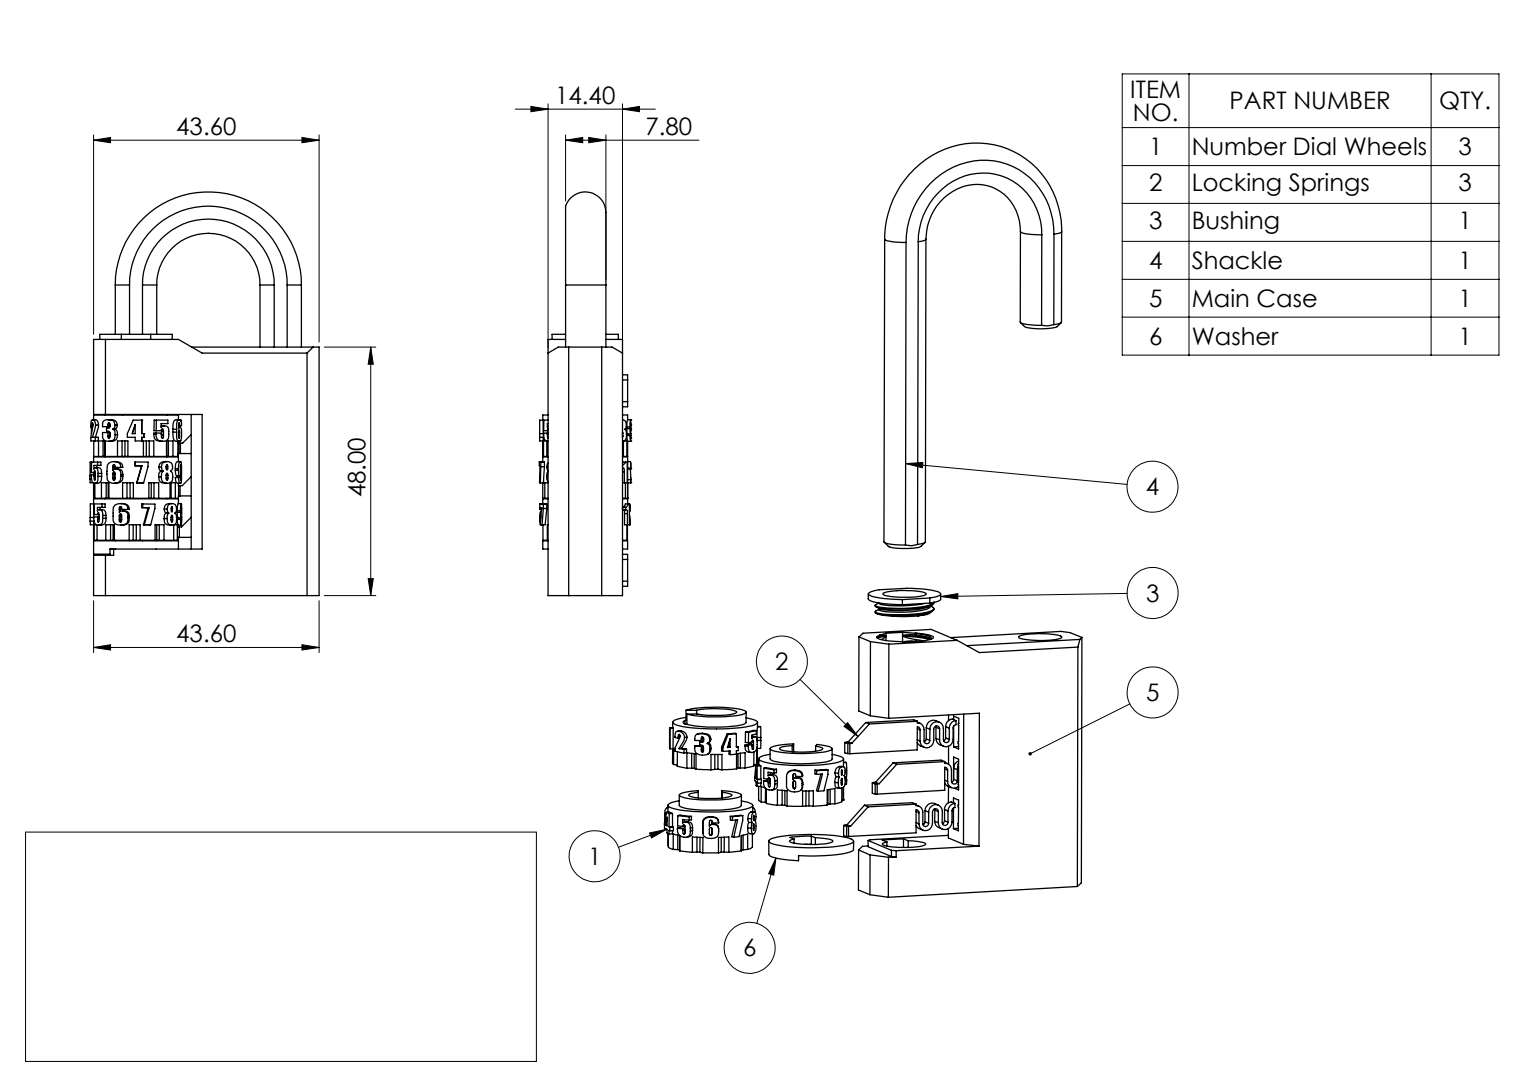
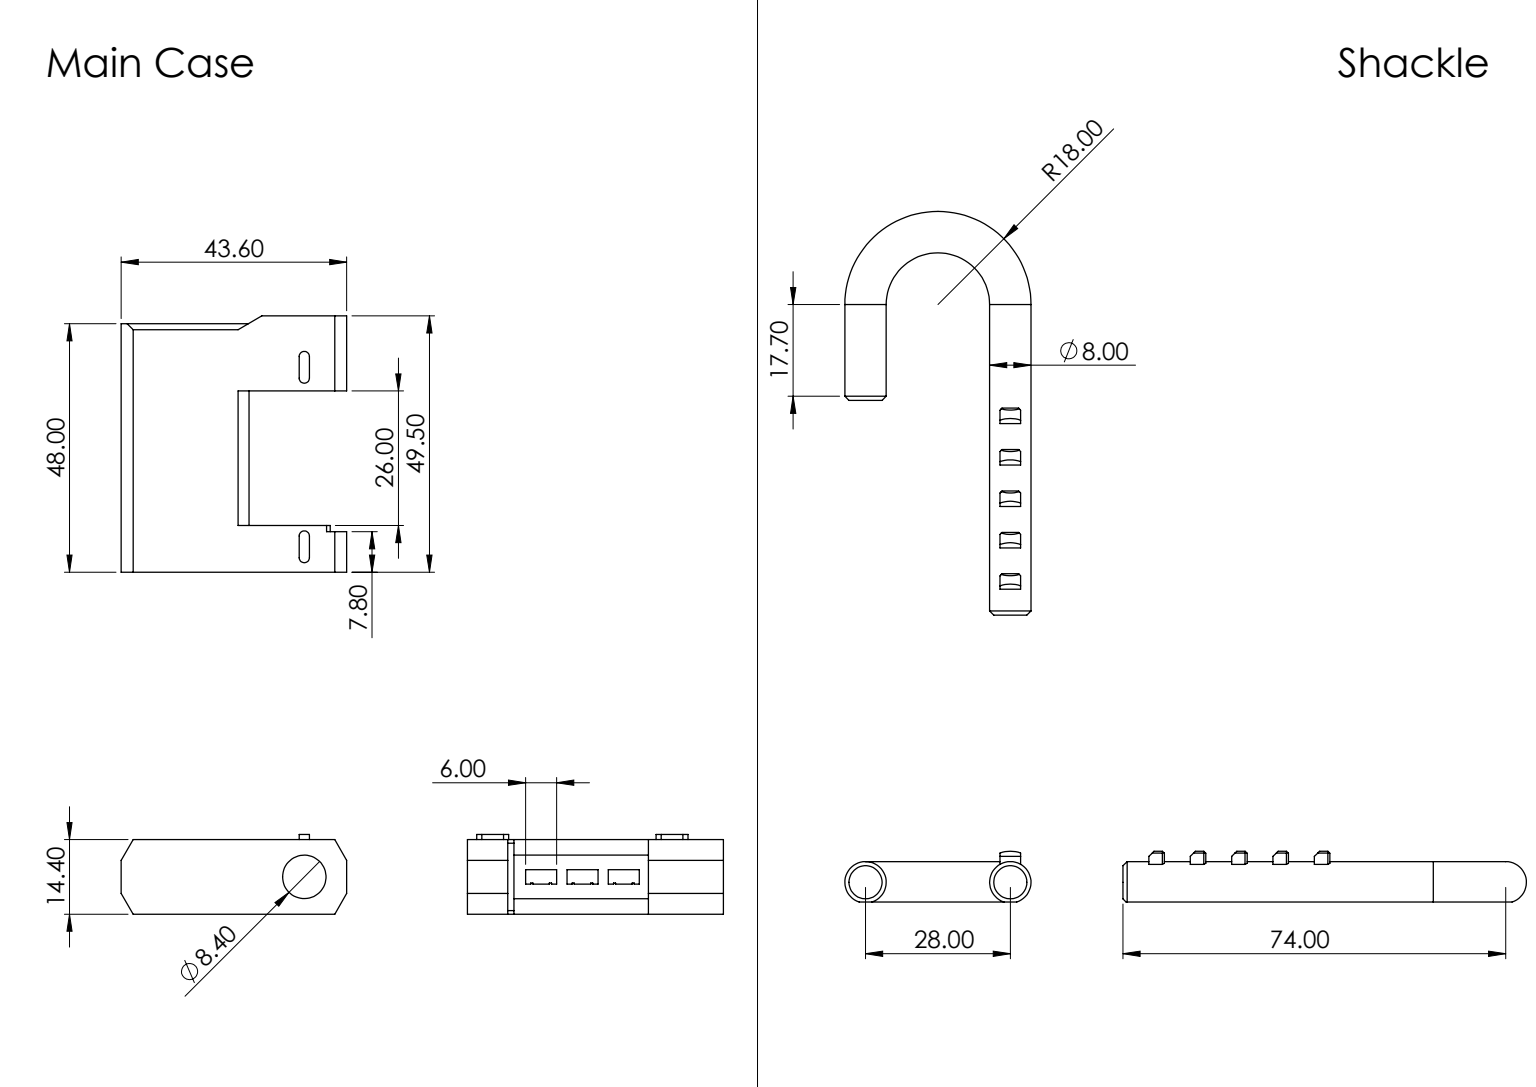
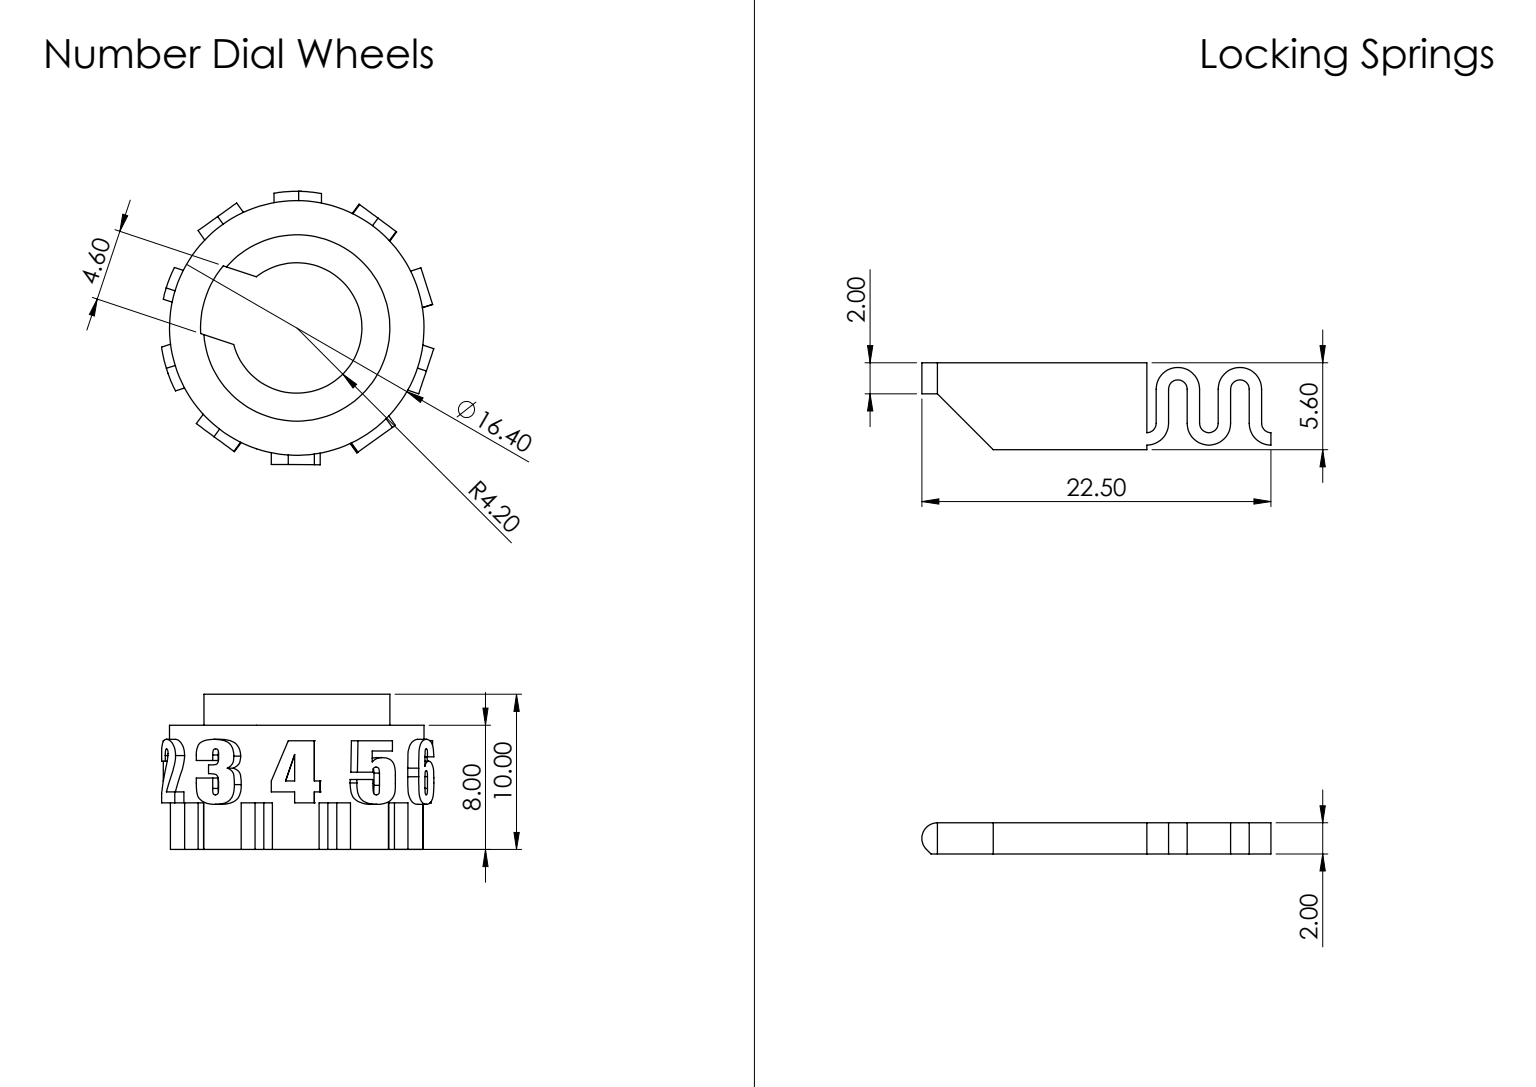
ISO-10303-21;
HEADER;
FILE_DESCRIPTION (('STEP AP214'),
    '1' );
FILE_NAME ('MAS-160',
    '2026-10-06T10:59:17',
    ( '' ),
    ( '' ),
    'SwSTEP 2.0',
    'SolidWorks 2026',
    '' );
FILE_SCHEMA (( 'AUTOMOTIVE_DESIGN' ));
ENDSEC;

DATA;
#1 = CARTESIAN_POINT ( 'NONE',  ( -5.668520211720758262, 50.55432463793220421, 79.06611278947218580 ) ) ;
#2 = EDGE_CURVE ( 'NONE', #13018, #165, #5489, .T. ) ;
#3 = DIRECTION ( 'NONE',  ( -0.007885122365275663500, -0.9999689119394085113, -1.805443505845543142E-16 ) ) ;
#4 = VECTOR ( 'NONE', #1471, 1000.000000000000000 ) ;
#5 = CIRCLE ( 'NONE', #15294, 8.199999999999995737 ) ;
#6 = CARTESIAN_POINT ( 'NONE',  ( -5.044287576081563529, 45.27497882680665242, 92.45433879953097289 ) ) ;
#7 = EDGE_CURVE ( 'NONE', #18543, #18148, #5615, .T. ) ;
#8 = EDGE_CURVE ( 'NONE', #10795, #13483, #5393, .T. ) ;
#9 = CARTESIAN_POINT ( 'NONE',  ( 9.261243355884198891, 42.55025836209524215, 77.91040118276930571 ) ) ;
#10 = ORIENTED_EDGE ( 'NONE', *, *, #4967, .T. ) ;
#11 = CARTESIAN_POINT ( 'NONE',  ( 0.5922110576113025493, 52.20739479508054615, 75.36022115247205022 ) ) ;
#12 = CARTESIAN_POINT ( 'NONE',  ( 4.579592178280777581, 52.10552964593085790, 78.58658920843723195 ) ) ;
#13 = CARTESIAN_POINT ( 'NONE',  ( -4.517072128342570991, 36.94403992325788977, 76.53375056423675460 ) ) ;
#14 = DIRECTION ( 'NONE',  ( -5.084437235940625660E-16, 1.000000000000000000, 0.000000000000000000 ) ) ;
#15 = CARTESIAN_POINT ( 'NONE',  ( 13.32277635493562684, 36.96218137147968008, 93.55433879953098142 ) ) ;
#16 = ORIENTED_EDGE ( 'NONE', *, *, #17837, .F. ) ;
#17 = CARTESIAN_POINT ( 'NONE',  ( -4.383821200644077543, 51.47232351541473605, 78.52322435057745054 ) ) ;
#18 = ORIENTED_EDGE ( 'NONE', *, *, #1917, .T. ) ;
#19 = CARTESIAN_POINT ( 'NONE',  ( 6.198496396448986090, 45.68315280215533392, 92.83621380123798872 ) ) ;
#20 = VECTOR ( 'NONE', #2644, 1000.000000000000000 ) ;
#21 = DIRECTION ( 'NONE',  ( -0.9534635866061492715, -0.3015081906286096181, -2.009271279954799034E-16 ) ) ;
#22 = DIRECTION ( 'NONE',  ( 1.000000000000000000, 1.402518428993831676E-16, 0.000000000000000000 ) ) ;
#23 = FACE_OUTER_BOUND ( 'NONE', #2715, .T. ) ;
#24 = PRODUCT_DEFINITION_SHAPE ( 'NONE', 'NONE',  #21038 ) ;
#25 = CARTESIAN_POINT ( 'NONE',  ( 11.22215374030650281, 42.76218137147968434, 61.80715055817104542 ) ) ;
#26 = VERTEX_POINT ( 'NONE', #13599 ) ;
#27 = CARTESIAN_POINT ( 'NONE',  ( 4.987972048783305468, 51.80387588613526617, 77.70137231118654597 ) ) ;
#28 = ORIENTED_EDGE ( 'NONE', *, *, #6498, .T. ) ;
#29 = DIRECTION ( 'NONE',  ( -1.402518428993831183E-16, 1.000000000000000000, -3.469446951953617640E-16 ) ) ;
#30 = EDGE_CURVE ( 'NONE', #19399, #15803, #16589, .T. ) ;
#31 = CARTESIAN_POINT ( 'NONE',  ( -4.567115856812060670, 47.10047254335474065, 90.96121380123797451 ) ) ;
#32 = PRODUCT_DEFINITION_FORMATION_WITH_SPECIFIED_SOURCE ( 'ANY', '', #540, .NOT_KNOWN. ) ;
#33 = DIRECTION ( 'NONE',  ( -1.000000000000000000, 0.000000000000000000, 0.000000000000000000 ) ) ;
#34 =( BOUNDED_CURVE ( )  B_SPLINE_CURVE ( 2, ( #7482, #18864, #675, #2170, #8669, #8881, #884, #11966, #2587, #10382, #10705 ),
 .UNSPECIFIED., .F., .F. ) 
 B_SPLINE_CURVE_WITH_KNOTS ( ( 3, 2, 2, 2, 2, 3 ),
 ( 0.5133705948588321855, 0.5208165094390924121, 0.5468573349110280590, 0.5728981603829637059, 0.5989389858548992418, 0.6196804601785050881 ),
 .UNSPECIFIED. ) 
 CURVE ( )  GEOMETRIC_REPRESENTATION_ITEM ( )  RATIONAL_B_SPLINE_CURVE ( ( 0.9689162004317901644, 0.9782346953885442398, 1.000000000000000000, 0.9238795325112867385, 1.000000000000000000, 0.9238795325112867385, 1.000000000000000000, 0.9238795325112867385, 1.000000000000000000, 0.9393701738211195362, 0.9753234597474376155 ) ) 
 REPRESENTATION_ITEM ( '' )  );
#35 = ORIENTED_EDGE ( 'NONE', *, *, #1554, .F. ) ;
#36 = DIRECTION ( 'NONE',  ( -0.5941461771851783702, -0.8043570849667693867, -2.357623395011398763E-16 ) ) ;
#37 = DIRECTION ( 'NONE',  ( 1.000000000000000000, 0.000000000000000000, 0.000000000000000000 ) ) ;
#38 = CARTESIAN_POINT ( 'NONE',  ( 5.756838674491786101, 51.23594508156129734, 75.97260389846793771 ) ) ;
#39 = CARTESIAN_POINT ( 'NONE',  ( -1.214884381343047881, 47.76843358786783966, 61.41730067788144964 ) ) ;
#40 = PLANE ( 'NONE',  #3794 ) ;
#41 = ORIENTED_EDGE ( 'NONE', *, *, #20258, .F. ) ;
#42 = CARTESIAN_POINT ( 'NONE',  ( -4.383767596367525776, 51.47236181906818331, 76.38961819735682468 ) ) ;
#43 = DIRECTION ( 'NONE',  ( -1.402518428993830937E-16, 1.000000000000000000, -3.469446951953617147E-16 ) ) ;
#44 = ORIENTED_EDGE ( 'NONE', *, *, #9004, .T. ) ;
#45 = CARTESIAN_POINT ( 'NONE',  ( 4.947340820402381212, 51.83388853781453776, 77.72408214165703555 ) ) ;
#46 = CARTESIAN_POINT ( 'NONE',  ( -7.770838052284047670, 41.18381739692070198, 76.59276269229415846 ) ) ;
#47 = FACE_OUTER_BOUND ( 'NONE', #1899, .T. ) ;
#48 = CARTESIAN_POINT ( 'NONE',  ( -3.467962453771610498, 40.50591351489412517, 91.93871379611699979 ) ) ;
#49 = VECTOR ( 'NONE', #11838, 1000.000000000000000 ) ;
#50 = CARTESIAN_POINT ( 'NONE',  ( -4.705149740856862550, 37.08296527939383935, 78.93669174070734584 ) ) ;
#51 = AXIS2_PLACEMENT_3D ( 'NONE', #3757, #13451, #252 ) ;
#52 = CARTESIAN_POINT ( 'NONE',  ( 11.22215374030650281, 45.56218137147968861, 78.80433879953099563 ) ) ;
#53 = CARTESIAN_POINT ( 'NONE',  ( -3.095340769291234473, 36.81869718614577636, 77.24173421363296654 ) ) ;
#54 = VERTEX_POINT ( 'NONE', #8619 ) ;
#55 = CARTESIAN_POINT ( 'NONE',  ( 27.03948732994508219, 45.16218137147969003, 73.00433879953099847 ) ) ;
#56 = CARTESIAN_POINT ( 'NONE',  ( -3.319090015466918064, 36.97315379936787849, 77.82155188814751057 ) ) ;
#57 = VERTEX_POINT ( 'NONE', #8931 ) ;
#58 = CARTESIAN_POINT ( 'NONE',  ( -8.080917653967048864, 42.28401339625642663, 76.87634113524943302 ) ) ;
#59 = DIRECTION ( 'NONE',  ( -0.5813877811927011807, 0.8136266022444372803, 5.636455622144619183E-17 ) ) ;
#60 = CARTESIAN_POINT ( 'NONE',  ( 9.342575031381675998, 42.79401455314646086, 78.75800315165874110 ) ) ;
#61 = ORIENTED_EDGE ( 'NONE', *, *, #4152, .T. ) ;
#62 = CARTESIAN_POINT ( 'NONE',  ( -1.876873622437039701, 39.01745058958429269, 93.96996379782397923 ) ) ;
#63 = CARTESIAN_POINT ( 'NONE',  ( -5.888951387225215939, 37.95739186912707197, 75.98496980016291502 ) ) ;
#64 = EDGE_LOOP ( 'NONE', ( #4003, #6865, #2890, #187 ) ) ;
#65 = CIRCLE ( 'NONE', #13313, 4.200000000000000178 ) ;
#66 = CARTESIAN_POINT ( 'NONE',  ( 11.22215374030649926, 45.56218137147968861, 78.80433879953099563 ) ) ;
#67 = CARTESIAN_POINT ( 'NONE',  ( 2.522153740306511072, 49.16218137147969003, 50.55433879953100273 ) ) ;
#68 = CARTESIAN_POINT ( 'NONE',  ( -0.8237052942265477018, 49.18499566818285018, 93.69558879953099506 ) ) ;
#69 = CIRCLE ( 'NONE', #12653, 8.199999999999999289 ) ;
#70 = ORIENTED_EDGE ( 'NONE', *, *, #17800, .F. ) ;
#71 = CARTESIAN_POINT ( 'NONE',  ( 4.142779209164833887, 51.51417078508897163, 78.58658920843723195 ) ) ;
#72 = CARTESIAN_POINT ( 'NONE',  ( -4.555118767358855791, 36.97214344288707366, 78.05402056118774112 ) ) ;
#73 = ORIENTED_EDGE ( 'NONE', *, *, #14534, .T. ) ;
#74 = CARTESIAN_POINT ( 'NONE',  ( -7.805021908755670701, 41.31633897062200589, 78.88165831555673435 ) ) ;
#75 = DIRECTION ( 'NONE',  ( 1.334402673828313339E-16, 1.871524341742854397E-32, -1.000000000000000000 ) ) ;
#76 = ADVANCED_FACE ( 'NONE', ( #16800 ), #11914, .T. ) ;
#77 = CARTESIAN_POINT ( 'NONE',  ( 2.122153740306496505, 47.82824192744437397, 69.55433879953100984 ) ) ;
#78 = AXIS2_PLACEMENT_3D ( 'NONE', #12417, #15502, #20488 ) ;
#79 = CARTESIAN_POINT ( 'NONE',  ( 0.3449000470298889676, 52.34510639596846460, 77.07502437766733294 ) ) ;
#80 = CARTESIAN_POINT ( 'NONE',  ( 0.5221537403065104055, 40.36218137147969998, 46.15433879953098284 ) ) ;
#81 = VECTOR ( 'NONE', #12886, 999.9999999999998863 ) ;
#82 = ORIENTED_EDGE ( 'NONE', *, *, #15786, .F. ) ;
#83 = CARTESIAN_POINT ( 'NONE',  ( -5.510184220575293779, 38.60782276366593635, 76.52855510524061344 ) ) ;
#84 = CARTESIAN_POINT ( 'NONE',  ( 9.340212240349364592, 42.78693311852996572, 76.09591779779900378 ) ) ;
#85 = CARTESIAN_POINT ( 'NONE',  ( 8.299662904660788598, 41.56403757284476796, 75.97198585835440099 ) ) ;
#86 = CARTESIAN_POINT ( 'NONE',  ( 1.695410614910025870, 52.88397731476800345, 79.31282343688214098 ) ) ;
#87 = ORIENTED_EDGE ( 'NONE', *, *, #18743, .F. ) ;
#88 = CARTESIAN_POINT ( 'NONE',  ( 5.873814141894775354, 51.14954001584995069, 78.86250487280319987 ) ) ;
#89 = ORIENTED_EDGE ( 'NONE', *, *, #15661, .F. ) ;
#90 = AXIS2_PLACEMENT_3D ( 'NONE', #13292, #19764, #11704 ) ;
#91 = VECTOR ( 'NONE', #3485, 1000.000000000000114 ) ;
#92 = CARTESIAN_POINT ( 'NONE',  ( 0.5221537403065010796, 44.16218137147969003, 54.55433879953099563 ) ) ;
#93 =( LENGTH_UNIT ( ) NAMED_UNIT ( * ) SI_UNIT ( .MILLI., .METRE. ) );
#94 = CARTESIAN_POINT ( 'NONE',  ( 5.077155773762835445, 37.34368029226138219, 77.47144026546204998 ) ) ;
#95 = ADVANCED_FACE ( 'NONE', ( #11803 ), #8817, .F. ) ;
#96 = LINE ( 'NONE', #16272, #3476 ) ;
#97 = CARTESIAN_POINT ( 'NONE',  ( 5.856396280011940014, 46.10368687828906076, 93.18871379782397923 ) ) ;
#98 = CARTESIAN_POINT ( 'NONE',  ( 32.52215374030649286, 44.16218137147969003, 105.5543387995310098 ) ) ;
#99 = CARTESIAN_POINT ( 'NONE',  ( 6.470280134917119064, 49.78412166693355800, 77.24227907682649175 ) ) ;
#100 = CARTESIAN_POINT ( 'NONE',  ( 4.485821066275814673, 51.34094918448491995, 77.76180969966527812 ) ) ;
#101 = CARTESIAN_POINT ( 'NONE',  ( 5.384092268968043271, 50.76532863195453160, 75.97198585835440099 ) ) ;
#102 = CARTESIAN_POINT ( 'NONE',  ( -3.350035803220276609, 49.20851703305431357, 90.72683880123797451 ) ) ;
#103 = ORIENTED_EDGE ( 'NONE', *, *, #5988, .T. ) ;
#104 = CARTESIAN_POINT ( 'NONE',  ( -5.234090592717892676, 38.40967907571953077, 79.34222993022952153 ) ) ;
#105 = AXIS2_PLACEMENT_3D ( 'NONE', #8174, #11698, #19756 ) ;
#106 = EDGE_CURVE ( 'NONE', #5849, #17982, #8716, .T. ) ;
#107 = CARTESIAN_POINT ( 'NONE',  ( 8.951227662965957066, 41.62112166339042574, 78.59502675972919405 ) ) ;
#108 = CARTESIAN_POINT ( 'NONE',  ( -4.895593109503404428, 37.22363812428621088, 78.53742703482498655 ) ) ;
#109 = CARTESIAN_POINT ( 'NONE',  ( -1.477846259693489150, 50.16218137147969713, 53.15433879953100416 ) ) ;
#110 = CARTESIAN_POINT ( 'NONE',  ( 8.529329397667178014, 40.35666579756309602, 75.60774188071792423 ) ) ;
#111 = EDGE_LOOP ( 'NONE', ( #358, #7162, #18029, #16335 ) ) ;
#112 = CARTESIAN_POINT ( 'NONE',  ( 0.5218139128070994337, 52.20794990243870615, 75.36134551364482093 ) ) ;
#113 = CARTESIAN_POINT ( 'NONE',  ( 4.611645699796032893, 52.08185300078213942, 78.81874598975664981 ) ) ;
#114 = CARTESIAN_POINT ( 'NONE',  ( 7.692705115657170190, 40.18434116893706687, 78.65627992829327297 ) ) ;
#115 = DIRECTION ( 'NONE',  ( -1.000000000000000000, 0.000000000000000000, 0.000000000000000000 ) ) ;
#116 = CARTESIAN_POINT ( 'NONE',  ( -2.244031111076484120, 49.10779090901081645, 92.45433879953095868 ) ) ;
#117 = ORIENTED_EDGE ( 'NONE', *, *, #13949, .F. ) ;
#118 = ADVANCED_FACE ( 'NONE', ( #19767 ), #15314, .F. ) ;
#119 = CARTESIAN_POINT ( 'NONE',  ( -4.541431855014749885, 51.35970071229581180, 78.93463757479271692 ) ) ;
#120 = EDGE_CURVE ( 'NONE', #5204, #4614, #20185, .T. ) ;
#121 = VECTOR ( 'NONE', #9015, 1000.000000000000000 ) ;
#122 = VERTEX_POINT ( 'NONE', #18600 ) ;
#123 = CARTESIAN_POINT ( 'NONE',  ( -3.981178359372548492, 46.76218137147973408, 95.41433880294498238 ) ) ;
#124 = CARTESIAN_POINT ( 'NONE',  ( 4.359773538758245692, 47.36728266200564263, 95.05433879953096721 ) ) ;
#125 = CARTESIAN_POINT ( 'NONE',  ( -7.372207198384979066, 41.95818682111052311, 78.62287654527649750 ) ) ;
#126 = EDGE_CURVE ( 'NONE', #1287, #15187, #18942, .T. ) ;
#127 = CARTESIAN_POINT ( 'NONE',  ( 8.647256388514012571, 43.05630782556218605, 78.60052408832618198 ) ) ;
#128 = ORIENTED_EDGE ( 'NONE', *, *, #19583, .F. ) ;
#129 = VERTEX_POINT ( 'NONE', #13492 ) ;
#130 = AXIS2_PLACEMENT_3D ( 'NONE', #14597, #8214, #5004 ) ;
#131 = CARTESIAN_POINT ( 'NONE',  ( -1.477846259693492481, 49.81903562097207327, 69.15433879953098995 ) ) ;
#132 = CARTESIAN_POINT ( 'NONE',  ( -5.154188915835984375, 42.64120994080404614, 91.11746380123797451 ) ) ;
#133 = CARTESIAN_POINT ( 'NONE',  ( -3.350035803220276609, 49.20851703305431357, 94.47683880123798872 ) ) ;
#134 = ORIENTED_EDGE ( 'NONE', *, *, #20923, .T. ) ;
#135 = DIRECTION ( 'NONE',  ( 1.000000000000000000, 0.000000000000000000, 0.000000000000000000 ) ) ;
#136 = CARTESIAN_POINT ( 'NONE',  ( -5.850799091716242017, 37.92921030530281001, 79.12851299606570876 ) ) ;
#137 = CARTESIAN_POINT ( 'NONE',  ( 4.483628625085211539, 47.60909685017714565, 92.55433879953102405 ) ) ;
#138 = LINE ( 'NONE', #1946, #11877 ) ;
#139 = DIRECTION ( 'NONE',  ( 5.626130192357176673E-16, 1.831515347669941892E-30, -1.000000000000000000 ) ) ;
#140 = VERTEX_POINT ( 'NONE', #614 ) ;
#141 = CARTESIAN_POINT ( 'NONE',  ( -4.572866156349838285, 51.33723891144499163, 75.97260225988416948 ) ) ;
#142 = CARTESIAN_POINT ( 'NONE',  ( 1.514255888186003984, 52.36218137147968577, 83.03825919817350609 ) ) ;
#143 = ORIENTED_EDGE ( 'NONE', *, *, #10138, .T. ) ;
#144 = CARTESIAN_POINT ( 'NONE',  ( 4.577379499810326990, 52.10716406238486087, 78.43496551412393103 ) ) ;
#145 = ADVANCED_FACE ( 'NONE', ( #13399 ), #7094, .T. ) ;
#146 = CARTESIAN_POINT ( 'NONE',  ( -7.419359026272076996, 40.07233033562560109, 78.47931198110067896 ) ) ;
#147 = CARTESIAN_POINT ( 'NONE',  ( -5.170918566808907713, 50.90989255502720567, 75.43678921887351407 ) ) ;
#148 = CARTESIAN_POINT ( 'NONE',  ( -3.134114116279072437, 48.15229756555780227, 92.87621379611699979 ) ) ;
#149 = CARTESIAN_POINT ( 'NONE',  ( -5.616286711741430793, 44.43019146960381960, 93.73558879782397923 ) ) ;
#150 = LINE ( 'NONE', #6632, #10274 ) ;
#151 = ADVANCED_FACE ( 'NONE', ( #2321 ), #726, .T. ) ;
#152 = CARTESIAN_POINT ( 'NONE',  ( 3.722852957781953798, 40.32059543431686421, 95.05433879953096721 ) ) ;
#153 = ADVANCED_FACE ( 'NONE', ( #834 ), #13296, .T. ) ;
#154 = CARTESIAN_POINT ( 'NONE',  ( -3.501255140781828423, 36.19369683415101946, 76.91456057462045237 ) ) ;
#155 = ORIENTED_EDGE ( 'NONE', *, *, #1332, .F. ) ;
#156 = CARTESIAN_POINT ( 'NONE',  ( 0.6393167648259392433, 52.21315491623544602, 79.54845644658969661 ) ) ;
#157 = LINE ( 'NONE', #5245, #2424 ) ;
#158 = VERTEX_POINT ( 'NONE', #10219 ) ;
#159 = DIRECTION ( 'NONE',  ( 0.9485903129789495791, -0.3165065846431930341, 8.934458285744763183E-17 ) ) ;
#160 = DIRECTION ( 'NONE',  ( 1.193617070626243484E-16, 1.000000000000000000, 0.000000000000000000 ) ) ;
#161 = DIRECTION ( 'NONE',  ( -1.779391786395883536E-16, -5.922860397471806844E-17, 1.000000000000000000 ) ) ;
#162 = ORIENTED_EDGE ( 'NONE', *, *, #19825, .F. ) ;
#163 = PLANE ( 'NONE',  #17008 ) ;
#164 = CARTESIAN_POINT ( 'NONE',  ( -5.460139946343538497, 38.57665262741940637, 76.06004113464240390 ) ) ;
#165 = VERTEX_POINT ( 'NONE', #16122 ) ;
#166 = DIRECTION ( 'NONE',  ( 1.000000000000000000, 0.000000000000000000, 0.000000000000000000 ) ) ;
#167 = CARTESIAN_POINT ( 'NONE',  ( 0.7308905865242323330, 52.95996087887004933, 76.81167861208460579 ) ) ;
#168 = PLANE ( 'NONE',  #8612 ) ;
#169 = EDGE_LOOP ( 'NONE', ( #1521, #15928, #6222, #1148 ) ) ;
#170 = DIRECTION ( 'NONE',  ( -4.731737692062685363E-17, 0.7071067811865536790, 0.7071067811865414665 ) ) ;
#171 = CARTESIAN_POINT ( 'NONE',  ( -4.853788242550869825, 37.19275855307108003, 77.90854597583356167 ) ) ;
#172 = ORIENTED_EDGE ( 'NONE', *, *, #6800, .T. ) ;
#173 = DIRECTION ( 'NONE',  ( 1.540237394707284220E-16, 1.793354297423764243E-16, -1.000000000000000000 ) ) ;
#174 = CARTESIAN_POINT ( 'NONE',  ( 5.506586839745581941, 50.67343267475700941, 78.88820493356335817 ) ) ;
#175 = CARTESIAN_POINT ( 'NONE',  ( 1.314047178454490705, 52.92828027204963348, 75.43137060453751985 ) ) ;
#176 = CARTESIAN_POINT ( 'NONE',  ( 2.043125170982144745, 38.48583871533720213, 95.02371380123798872 ) ) ;
#177 = CARTESIAN_POINT ( 'NONE',  ( -43.61452724460164632, 45.75098584416670633, -16.20000000000000284 ) ) ;
#178 = EDGE_CURVE ( 'NONE', #3564, #14970, #12223, .T. ) ;
#179 = CARTESIAN_POINT ( 'NONE',  ( -4.518988042728760313, 37.69480848959909025, 76.08971211654539957 ) ) ;
#180 = CARTESIAN_POINT ( 'NONE',  ( 0.8326822781444389587, 52.96411479610753759, 76.79008513575435302 ) ) ;
#181 = CARTESIAN_POINT ( 'NONE',  ( 4.121594020068452657, 36.83821297622463220, 75.83703142516586126 ) ) ;
#182 = ORIENTED_EDGE ( 'NONE', *, *, #1186, .F. ) ;
#183 = DIRECTION ( 'NONE',  ( -1.000000000000000000, -3.942553354492745503E-16, 0.000000000000000000 ) ) ;
#184 = DIRECTION ( 'NONE',  ( 0.3165065846431826535, 0.9485903129789529098, 2.188653791613874008E-16 ) ) ;
#185 = LINE ( 'NONE', #9890, #14702 ) ;
#186 = CARTESIAN_POINT ( 'NONE',  ( 6.712139372526147341, 50.53030293778272863, 77.80505143490314879 ) ) ;
#187 = ORIENTED_EDGE ( 'NONE', *, *, #7159, .F. ) ;
#188 = VERTEX_POINT ( 'NONE', #4227 ) ;
#189 = CARTESIAN_POINT ( 'NONE',  ( 2.263363662449282110, 49.77488197367689793, 93.03606768333816035 ) ) ;
#190 = EDGE_LOOP ( 'NONE', ( #6563, #851, #9237, #15797, #220 ) ) ;
#191 = EDGE_CURVE ( 'NONE', #225, #12203, #12716, .T. ) ;
#192 = CARTESIAN_POINT ( 'NONE',  ( 7.680545890134844456, 40.16247990082648300, 76.65742129588737441 ) ) ;
#193 = PLANE ( 'NONE',  #3154 ) ;
#194 = DIRECTION ( 'NONE',  ( -0.000000000000000000, -0.000000000000000000, 1.000000000000000000 ) ) ;
#195 = CARTESIAN_POINT ( 'NONE',  ( 4.673174852049362116, 39.63213674411673537, 92.95433879782399345 ) ) ;
#196 = DIRECTION ( 'NONE',  ( 0.000000000000000000, 1.000000000000000000, 0.000000000000000000 ) ) ;
#197 = CARTESIAN_POINT ( 'NONE',  ( 4.102313797646099047, 51.53324301277321240, 76.36737811492949390 ) ) ;
#199 = DIRECTION ( 'NONE',  ( -0.000000000000000000, -0.000000000000000000, 1.000000000000000000 ) ) ;
#198 = B_SPLINE_CURVE_WITH_KNOTS ( 'NONE', 3,
 ( #12240, #12351, #18723, #2450, #1065, #10868, #10667, #18831, #17129, #9158, #17339, #4238, #15432 ),
 .UNSPECIFIED., .F., .F.,
 ( 4, 1, 1, 1, 1, 1, 1, 1, 1, 1, 4 ),
 ( 0.000000000000000000, 0.08953921432355217702, 0.1742669454086417657, 0.2528767480256390865, 0.3294736160795620483, 0.4632125218299475988, 0.5712501803543521550, 0.6337422670347153675, 0.7254863994935087934, 0.8484041168876338412, 0.9999999999999998890 ),
 .UNSPECIFIED. ) ;
#200 = LINE ( 'NONE', #5090, #121 ) ;
#201 = CARTESIAN_POINT ( 'NONE',  ( 2.043125170982144745, 38.48583871533720213, 93.77371380123798872 ) ) ;
#202 = ORIENTED_EDGE ( 'NONE', *, *, #9221, .T. ) ;
#203 = LINE ( 'NONE', #6687, #3751 ) ;
#204 = FACE_OUTER_BOUND ( 'NONE', #1503, .T. ) ;
#205 = CARTESIAN_POINT ( 'NONE',  ( 5.347971804495873727, 50.79179859581513057, 78.93139168979107012 ) ) ;
#206 = EDGE_CURVE ( 'NONE', #17910, #5649, #11129, .T. ) ;
#207 = FACE_OUTER_BOUND ( 'NONE', #16478, .T. ) ;
#208 = DIRECTION ( 'NONE',  ( -0.5813877811927012917, 0.8136266022444372803, 5.636455622144620416E-17 ) ) ;
#209 = SHAPE_REPRESENTATION ( 'Shackle', ( #18366 ), #4082 ) ;
#210 = ORIENTED_EDGE ( 'NONE', *, *, #3657, .F. ) ;
#211 = CARTESIAN_POINT ( 'NONE',  ( 6.223727862608700256, 38.34032085607169904, 75.70392102816973079 ) ) ;
#212 = CARTESIAN_POINT ( 'NONE',  ( 0.5221537403065045213, 39.16218137147969003, 94.60386871425484401 ) ) ;
#213 = CARTESIAN_POINT ( 'NONE',  ( -3.510185363184279428, 36.20029322970840724, 76.30596599901106458 ) ) ;
#214 = CARTESIAN_POINT ( 'NONE',  ( -4.348661956197086731, 37.56557963644259956, 78.93669174070734584 ) ) ;
#215 = ORIENTED_EDGE ( 'NONE', *, *, #16170, .F. ) ;
#216 = CARTESIAN_POINT ( 'NONE',  ( -4.405821937837398394, 51.45660259411479132, 78.79092181577959764 ) ) ;
#217 = VECTOR ( 'NONE', #7066, 1000.000000000000000 ) ;
#218 = DIRECTION ( 'NONE',  ( 0.000000000000000000, 0.000000000000000000, 1.000000000000000000 ) ) ;
#219 = EDGE_CURVE ( 'NONE', #16835, #11136, #4609, .T. ) ;
#220 = ORIENTED_EDGE ( 'NONE', *, *, #14561, .T. ) ;
#221 = CARTESIAN_POINT ( 'NONE',  ( 6.102441102155617969, 43.42752260303680600, 94.86746380294499659 ) ) ;
#222 = CARTESIAN_POINT ( 'NONE',  ( 2.099220375572687036, 52.20172610552850756, 77.53128952716078004 ) ) ;
#223 = CARTESIAN_POINT ( 'NONE',  ( 31.22215374030650281, 42.76218137147968434, 78.80433879953099563 ) ) ;
#224 = CARTESIAN_POINT ( 'NONE',  ( 31.03948732994507864, 43.16218137147969003, 76.90433879953100416 ) ) ;
#225 = VERTEX_POINT ( 'NONE', #1542 ) ;
#226 = DIRECTION ( 'NONE',  ( 1.540237394707284220E-16, 1.793354297423764243E-16, -1.000000000000000000 ) ) ;
#227 = ORIENTED_EDGE ( 'NONE', *, *, #2629, .T. ) ;
#228 = AXIS2_PLACEMENT_3D ( 'NONE', #7472, #20221, #2262 ) ;
#229 = CARTESIAN_POINT ( 'NONE',  ( 0.3201111382462868971, 51.36399839264385037, 76.44919174070734869 ) ) ;
#230 = DIRECTION ( 'NONE',  ( 1.134288711164059445E-16, 1.000000000000000000, 7.183611964723549989E-17 ) ) ;
#231 = CARTESIAN_POINT ( 'NONE',  ( -4.524181921268124462, 40.28999182795290324, 94.78933880123798872 ) ) ;
#232 = ORIENTED_EDGE ( 'NONE', *, *, #11068, .T. ) ;
#233 = CYLINDRICAL_SURFACE ( 'NONE', #6902, 4.999999999999997335 ) ;
#234 = CARTESIAN_POINT ( 'NONE',  ( 30.92220646078100188, 42.96218137147968008, 57.80715055817105252 ) ) ;
#235 = CARTESIAN_POINT ( 'NONE',  ( 5.175615907322522524, 46.72245102501825897, 92.55433879953095300 ) ) ;
#236 = CARTESIAN_POINT ( 'NONE',  ( -4.385374315297738690, 51.47121371654639432, 78.59092584394873882 ) ) ;
#237 = CARTESIAN_POINT ( 'NONE',  ( -0.3594811632358363429, 49.16218137147969003, 93.07733169107483207 ) ) ;
#238 = ORIENTED_EDGE ( 'NONE', *, *, #14421, .F. ) ;
#239 = CARTESIAN_POINT ( 'NONE',  ( 4.432284427945813121, 36.14044538431356557, 77.43080938776617472 ) ) ;
#240 = ORIENTED_EDGE ( 'NONE', *, *, #5848, .T. ) ;
#241 = LINE ( 'NONE', #6730, #1600 ) ;
#242 = LINE ( 'NONE', #11753, #2979 ) ;
#243 = CARTESIAN_POINT ( 'NONE',  ( 2.522153740306509295, 47.62628298661744708, 61.15433879953099705 ) ) ;
#244 = FACE_OUTER_BOUND ( 'NONE', #17677, .T. ) ;
#245 = AXIS2_PLACEMENT_3D ( 'NONE', #9767, #1571, #19535 ) ;
#246 = CARTESIAN_POINT ( 'NONE',  ( 6.660594192354429843, 43.89417127335556046, 93.11058879782397923 ) ) ;
#247 = CARTESIAN_POINT ( 'NONE',  ( 5.786794573647632944, 37.10832874265046399, 76.01697444493925104 ) ) ;
#248 = DIRECTION ( 'NONE',  ( 1.000000000000000000, -1.110223024625156540E-16, 1.779391786395883043E-16 ) ) ;
#249 = CARTESIAN_POINT ( 'NONE',  ( -3.906146384357795043, 51.81365245034167799, 75.48713596493043099 ) ) ;
#250 = ORIENTED_EDGE ( 'NONE', *, *, #19232, .F. ) ;
#251 = DIRECTION ( 'NONE',  ( 1.000000000000000000, 0.000000000000000000, 0.000000000000000000 ) ) ;
#252 = DIRECTION ( 'NONE',  ( 0.3165065846431827645, 0.9485903129789529098, 0.000000000000000000 ) ) ;
#253 = EDGE_CURVE ( 'NONE', #3468, #18406, #1056, .T. ) ;
#254 = AXIS2_PLACEMENT_3D ( 'NONE', #16070, #11180, #9791 ) ;
#255 = ORIENTED_EDGE ( 'NONE', *, *, #13064, .T. ) ;
#256 = DIRECTION ( 'NONE',  ( -1.000000000000000000, 0.000000000000000000, 0.000000000000000000 ) ) ;
#257 = ADVANCED_FACE ( 'NONE', ( #1439 ), #7307, .T. ) ;
#258 = CARTESIAN_POINT ( 'NONE',  ( -1.477846259693481601, 49.81903562097206617, 123.5543387995310098 ) ) ;
#259 = CARTESIAN_POINT ( 'NONE',  ( -0.8237052942265477018, 49.18499566818285018, 93.69558879953099506 ) ) ;
#260 = CARTESIAN_POINT ( 'NONE',  ( -7.560113746301722060, 42.96559675774617659, 76.25640820822667365 ) ) ;
#261 = ORIENTED_EDGE ( 'NONE', *, *, #19498, .F. ) ;
#262 = CARTESIAN_POINT ( 'NONE',  ( -2.939085670389444793, 51.59587639763223166, 75.45433879953088763 ) ) ;
#263 = CARTESIAN_POINT ( 'NONE',  ( -5.955451856753751549, 38.00651308716548726, 76.73301527011911105 ) ) ;
#264 = VERTEX_POINT ( 'NONE', #11855 ) ;
#265 = VECTOR ( 'NONE', #12060, 1000.000000000000000 ) ;
#266 = DIRECTION ( 'NONE',  ( -5.626130192357176673E-16, -1.831515347669941892E-30, 1.000000000000000000 ) ) ;
#267 = CARTESIAN_POINT ( 'NONE',  ( -4.517374237173717333, 36.94426307888177519, 76.44623874561141008 ) ) ;
#268 = EDGE_CURVE ( 'NONE', #10025, #14733, #19817, .T. ) ;
#269 = CARTESIAN_POINT ( 'NONE',  ( 5.025485839985549319, 41.56218137147963887, 93.22683879953099506 ) ) ;
#270 = ADVANCED_FACE ( 'NONE', ( #47 ), #9957, .F. ) ;
#271 = VERTEX_POINT ( 'NONE', #6526 ) ;
#272 = CARTESIAN_POINT ( 'NONE',  ( 27.63948732994508717, 36.35905713404685002, 74.70433879953098710 ) ) ;
#273 = ORIENTED_EDGE ( 'NONE', *, *, #5878, .F. ) ;
#274 = CARTESIAN_POINT ( 'NONE',  ( 1.799688516650707726, 52.86918891857825287, 75.67226899599502588 ) ) ;
#275 = VECTOR ( 'NONE', #4873, 1000.000000000000227 ) ;
#276 = DIRECTION ( 'NONE',  ( -1.110223024625156540E-16, -1.000000000000000000, -5.922860397471808077E-17 ) ) ;
#277 = CARTESIAN_POINT ( 'NONE',  ( 5.035970566151715566, 36.57181739631530348, 75.46362501775257670 ) ) ;
#278 = FACE_OUTER_BOUND ( 'NONE', #7758, .T. ) ;
#279 = VERTEX_POINT ( 'NONE', #19605 ) ;
#280 = CARTESIAN_POINT ( 'NONE',  ( -1.677846259693499542, 50.36218137147968577, 37.95170767603170248 ) ) ;
#281 = CARTESIAN_POINT ( 'NONE',  ( 8.494230864814916515, 42.61589131850842449, 75.57016332177543916 ) ) ;
#282 = DIRECTION ( 'NONE',  ( -1.000000000000000000, 0.000000000000000000, 0.000000000000000000 ) ) ;
#283 = CARTESIAN_POINT ( 'NONE',  ( 0.6452163281857689059, 52.96132085210302165, 79.54845644658969661 ) ) ;
#284 = ORIENTED_EDGE ( 'NONE', *, *, #126, .T. ) ;
#285 = VECTOR ( 'NONE', #15681, 1000.000000000000000 ) ;
#286 = ORIENTED_EDGE ( 'NONE', *, *, #14335, .T. ) ;
#287 = EDGE_CURVE ( 'NONE', #4528, #3672, #19715, .T. ) ;
#288 = CARTESIAN_POINT ( 'NONE',  ( 0.8455950101471356728, 52.35579997042385259, 72.45433879953087342 ) ) ;
#289 = EDGE_LOOP ( 'NONE', ( #6284, #6972, #19822, #1456 ) ) ;
#290 = CARTESIAN_POINT ( 'NONE',  ( -3.522017727535923459, 36.20903332061825353, 77.14704031750767399 ) ) ;
#291 = CARTESIAN_POINT ( 'NONE',  ( 6.434241825184708219, 49.81074171462121569, 75.93520998463665705 ) ) ;
#292 = CARTESIAN_POINT ( 'NONE',  ( 9.351996896326966180, 42.82225248009945773, 76.45750776978282204 ) ) ;
#293 = CARTESIAN_POINT ( 'NONE',  ( 24.32215374030650068, 44.16218137147968292, 45.55433879953098852 ) ) ;
#294 = DIRECTION ( 'NONE',  ( 0.3015081906286096181, -0.9534635866061492715, -1.245503830460495705E-16 ) ) ;
#295 = FACE_OUTER_BOUND ( 'NONE', #12710, .T. ) ;
#296 = CARTESIAN_POINT ( 'NONE',  ( -3.628867371436363953, 48.69222599884265179, 93.57933879782396502 ) ) ;
#297 = CARTESIAN_POINT ( 'NONE',  ( -5.784195910403845176, 44.99242805365518194, 93.38308880123807398 ) ) ;
#298 = CARTESIAN_POINT ( 'NONE',  ( 6.934807254081542638, 50.36582714328714871, 76.18099276316716839 ) ) ;
#299 = DIRECTION ( 'NONE',  ( 1.000000000000000000, 1.213411507412056509E-16, 0.000000000000000000 ) ) ;
#300 = LINE ( 'NONE', #12868, #1303 ) ;
#301 = CARTESIAN_POINT ( 'NONE',  ( 6.198496396448986090, 45.68315280215533392, 92.83621380123798872 ) ) ;
#302 = CIRCLE ( 'NONE', #9823, 6.000000000000002665 ) ;
#303 = CARTESIAN_POINT ( 'NONE',  ( -0.3080929418689875576, 37.85583172076933778, 92.44558880123798872 ) ) ;
#304 = ORIENTED_EDGE ( 'NONE', *, *, #20230, .T. ) ;
#305 = CARTESIAN_POINT ( 'NONE',  ( -4.006646489220814011, 48.09791109810387155, 82.45433879953087342 ) ) ;
#306 = CARTESIAN_POINT ( 'NONE',  ( 8.949918141112842562, 41.61719694332212072, 78.74360054667872078 ) ) ;
#307 = CARTESIAN_POINT ( 'NONE',  ( -4.873991315592625995, 37.20768174929765593, 78.81125587425833601 ) ) ;
#308 = CARTESIAN_POINT ( 'NONE',  ( 8.375041524787441460, 41.81431093369050700, 77.18036020728871449 ) ) ;
#309 = CARTESIAN_POINT ( 'NONE',  ( -1.883296302981685599, 36.95289499283964574, 72.45432679953087529 ) ) ;
#310 = CARTESIAN_POINT ( 'NONE',  ( 9.304727838458644484, 42.68058411497499804, 77.77798975163413786 ) ) ;
#311 = ORIENTED_EDGE ( 'NONE', *, *, #5198, .F. ) ;
#312 = ORIENTED_EDGE ( 'NONE', *, *, #19961, .F. ) ;
#313 = VECTOR ( 'NONE', #14999, 1000.000000000000114 ) ;
#314 = CARTESIAN_POINT ( 'NONE',  ( -4.884656273474451638, 44.39824779480852612, 94.28246379611698558 ) ) ;
#315 = CARTESIAN_POINT ( 'NONE',  ( 6.882736312352589536, 37.89144858414100270, 77.26022115247205591 ) ) ;
#316 = CARTESIAN_POINT ( 'NONE',  ( -1.183761187420877548, 49.81017696809242068, 83.28180655319408743 ) ) ;
#317 = CARTESIAN_POINT ( 'NONE',  ( -7.367656984315425817, 48.05973018190410073, 78.32492703482499508 ) ) ;
#318 = ORIENTED_EDGE ( 'NONE', *, *, #10196, .T. ) ;
#319 = CARTESIAN_POINT ( 'NONE',  ( 8.354092538887906372, 41.75152549397071766, 76.05553801048951357 ) ) ;
#320 = CARTESIAN_POINT ( 'NONE',  ( -4.517608495228999210, 36.94443611587072240, 78.61392107264721574 ) ) ;
#321 = AXIS2_PLACEMENT_3D ( 'NONE', #17043, #16440, #10161 ) ;
#322 = ORIENTED_EDGE ( 'NONE', *, *, #16808, .F. ) ;
#323 = CARTESIAN_POINT ( 'NONE',  ( 1.352400422481993658, 50.46853102219002096, 91.82058880123801714 ) ) ;
#324 = EDGE_CURVE ( 'NONE', #3856, #5035, #17993, .T. ) ;
#325 = CARTESIAN_POINT ( 'NONE',  ( 5.561379608955574483, 51.38032281970146897, 76.39036821129558064 ) ) ;
#326 = CARTESIAN_POINT ( 'NONE',  ( -3.147752837274839788, 36.84659392771992970, 78.05869123030269918 ) ) ;
#327 = CARTESIAN_POINT ( 'NONE',  ( -0.9988176903691428077, 49.83852402762217082, 95.64871380123798872 ) ) ;
#328 = AXIS2_PLACEMENT_3D ( 'NONE', #19020, #17738, #3059 ) ;
#329 = VECTOR ( 'NONE', #13331, 1000.000000000000114 ) ;
#330 = DIRECTION ( 'NONE',  ( -1.402518428993831676E-16, 1.000000000000000000, -0.000000000000000000 ) ) ;
#331 = ORIENTED_EDGE ( 'NONE', *, *, #15896, .T. ) ;
#332 = DIRECTION ( 'NONE',  ( 1.000000000000000000, 0.000000000000000000, 0.000000000000000000 ) ) ;
#333 = SHAPE_REPRESENTATION ( 'Main Case', ( #18366 ), #20720 ) ;
#334 = ORIENTED_EDGE ( 'NONE', *, *, #12574, .F. ) ;
#335 = AXIS2_PLACEMENT_3D ( 'NONE', #10924, #9219, #1536 ) ;
#336 = LINE ( 'NONE', #13015, #329 ) ;
#337 = CARTESIAN_POINT ( 'NONE',  ( 0.5221537403065064087, 48.16218137147969003, 82.55433879953099563 ) ) ;
#338 = EDGE_LOOP ( 'NONE', ( #4433, #13539, #17360, #8721, #20536, #4730 ) ) ;
#339 = DIRECTION ( 'NONE',  ( 1.540237394707284220E-16, 1.793354297423764243E-16, -1.000000000000000000 ) ) ;
#340 = CARTESIAN_POINT ( 'NONE',  ( 8.025296824724655664, 41.22723296074632060, 75.38759329643264095 ) ) ;
#341 = CARTESIAN_POINT ( 'NONE',  ( 5.829595689320886009, 51.18220240553836931, 75.98827401121828018 ) ) ;
#342 = LINE ( 'NONE', #6831, #16623 ) ;
#343 = CARTESIAN_POINT ( 'NONE',  ( 0.4259372535303960206, 52.96683778999253178, 78.89168391585492657 ) ) ;
#344 = ORIENTED_EDGE ( 'NONE', *, *, #19982, .T. ) ;
#345 = VECTOR ( 'NONE', #5616, 1000.000000000000000 ) ;
#346 = CARTESIAN_POINT ( 'NONE',  ( -4.032216884946988600, 50.97665165413603461, 76.31459635612003467 ) ) ;
#347 = VERTEX_POINT ( 'NONE', #243 ) ;
#348 = CARTESIAN_POINT ( 'NONE',  ( 7.860711257786343609, 47.82081138319720282, 79.44551527011911674 ) ) ;
#349 = LINE ( 'NONE', #9955, #14871 ) ;
#350 = CARTESIAN_POINT ( 'NONE',  ( -4.615868704430273084, 50.38673528273210422, 75.40305853716382956 ) ) ;
#351 = CARTESIAN_POINT ( 'NONE',  ( -3.467962453771611830, 40.50591351489412517, 93.18871379611699979 ) ) ;
#352 = FACE_OUTER_BOUND ( 'NONE', #4295, .T. ) ;
#353 = AXIS2_PLACEMENT_3D ( 'NONE', #1504, #7884, #14371 ) ;
#354 = EDGE_CURVE ( 'NONE', #13475, #8370, #13216, .T. ) ;
#355 = CARTESIAN_POINT ( 'NONE',  ( -1.419351766502866541, 49.49642391118513274, 91.15746379782397923 ) ) ;
#356 = CARTESIAN_POINT ( 'NONE',  ( 8.356924487248303279, 46.61990428187149149, 75.44110882394862472 ) ) ;
#357 = CARTESIAN_POINT ( 'NONE',  ( -7.655299514379396264, 47.45321114378259608, 78.28954034321952804 ) ) ;
#358 = ORIENTED_EDGE ( 'NONE', *, *, #20772, .T. ) ;
#359 = CARTESIAN_POINT ( 'NONE',  ( 1.029933359059799880, 52.96274971666686326, 79.52671882365912381 ) ) ;
#360 = CARTESIAN_POINT ( 'NONE',  ( -5.522333806888472196, 37.68658623078928116, 79.43312132436682305 ) ) ;
#361 = CARTESIAN_POINT ( 'NONE',  ( 11.22215374030650281, 42.96218137147968008, 69.40574467885102194 ) ) ;
#362 = ORIENTED_EDGE ( 'NONE', *, *, #3216, .T. ) ;
#363 = FACE_OUTER_BOUND ( 'NONE', #15901, .T. ) ;
#364 = EDGE_CURVE ( 'NONE', #7324, #12818, #18229, .T. ) ;
#365 = CARTESIAN_POINT ( 'NONE',  ( -1.677846259693482001, 44.16218137147969003, 56.15433879953099705 ) ) ;
#366 = CARTESIAN_POINT ( 'NONE',  ( -2.077846259693550746, 39.65884927180063357, 91.66433879953099506 ) ) ;
#367 = B_SPLINE_SURFACE_WITH_KNOTS ( 'NONE', 3, 1, ( 
 ( #9391, #8386 ),
 ( #3379, #9895 ),
 ( #13285, #7780 ),
 ( #14663, #17963 ),
 ( #16375, #15875 ),
 ( #88, #1696 ),
 ( #14261, #17467 ),
 ( #2891, #20742 ),
 ( #6177, #12681 ),
 ( #1292, #6570 ),
 ( #2001, #5180 ) ),
 .UNSPECIFIED., .F., .F., .F.,
 ( 4, 1, 1, 1, 1, 1, 1, 1, 4 ),
 ( 2, 2 ),
 ( 0.000000000000000000, 0.1116983415361904319, 0.2084596166200352318, 0.2965296202300037876, 0.3842340601578678183, 0.4893760538913073388, 0.6260801343201788383, 0.7954079187270842732, 1.000000000000000000 ),
 ( 0.000000000000000000, 1.000000000000000000 ),
 .UNSPECIFIED. ) ;
#368 = ORIENTED_EDGE ( 'NONE', *, *, #3626, .T. ) ;
#369 = CARTESIAN_POINT ( 'NONE',  ( -6.647464070959230753, 48.14170149837703860, 75.45433879953088763 ) ) ;
#371 = EDGE_CURVE ( 'NONE', #5117, #5383, #6092, .T. ) ;
#370 = ORIENTED_EDGE ( 'NONE', *, *, #9504, .F. ) ;
#372 = CYLINDRICAL_SURFACE ( 'NONE', #19299, 4.200000000000003730 ) ;
#373 = CARTESIAN_POINT ( 'NONE',  ( 0.5493427850443924898, 52.96217785025373104, 75.97284715006453837 ) ) ;
#374 = VERTEX_POINT ( 'NONE', #1646 ) ;
#375 = CARTESIAN_POINT ( 'NONE',  ( -4.311513864721317368, 37.56696343308806973, 77.92992558049613194 ) ) ;
#376 = CARTESIAN_POINT ( 'NONE',  ( 6.102441102155617969, 43.42752260303680600, 90.80496379953099506 ) ) ;
#377 = ORIENTED_EDGE ( 'NONE', *, *, #20663, .T. ) ;
#378 = CARTESIAN_POINT ( 'NONE',  ( 0.7854852052231534598, 52.35796933930620156, 77.46569646384521945 ) ) ;
#379 = CARTESIAN_POINT ( 'NONE',  ( 2.122153740306508496, 50.16218137147969713, 77.55433879953099563 ) ) ;
#380 = ADVANCED_FACE ( 'NONE', ( #1859 ), #12576, .T. ) ;
#381 = AXIS2_PLACEMENT_3D ( 'NONE', #1625, #19694, #14599 ) ;
#382 = ADVANCED_FACE ( 'NONE', ( #8446 ), #459, .F. ) ;
#383 = ADVANCED_FACE ( 'NONE', ( #16643 ), #2062, .T. ) ;
#384 = FACE_OUTER_BOUND ( 'NONE', #4989, .T. ) ;
#385 = PRODUCT_DEFINITION ( 'UNKNOWN', '', #13627, #8947 ) ;
#386 = CARTESIAN_POINT ( 'NONE',  ( -7.208272791143412128, 41.42712212161580254, 78.48592181560817949 ) ) ;
#387 = ORIENTED_EDGE ( 'NONE', *, *, #17284, .F. ) ;
#388 = ORIENTED_EDGE ( 'NONE', *, *, #1554, .T. ) ;
#389 = EDGE_CURVE ( 'NONE', #13884, #12946, #15257, .T. ) ;
#390 = DIRECTION ( 'NONE',  ( -2.267473790562806355E-16, 5.922860397471811774E-17, -1.000000000000000000 ) ) ;
#391 = CARTESIAN_POINT ( 'NONE',  ( 8.392124750090893315, 39.94545476467643397, 78.58253683706189463 ) ) ;
#392 = ORIENTED_EDGE ( 'NONE', *, *, #17307, .F. ) ;
#393 = VECTOR ( 'NONE', #11426, 1000.000000000000000 ) ;
#394 = CARTESIAN_POINT ( 'NONE',  ( 26.43948732994507367, 45.16218137147968292, 74.70433879953098710 ) ) ;
#395 = DIRECTION ( 'NONE',  ( -0.3165065846431827645, -0.9485903129789529098, 0.000000000000000000 ) ) ;
#396 = CARTESIAN_POINT ( 'NONE',  ( 3.460444912181559474, 49.25145096859824889, 94.39871380123798872 ) ) ;
#397 = PRESENTATION_LAYER_ASSIGNMENT (  '', '', ( #7877 ) ) ;
#398 = ORIENTED_EDGE ( 'NONE', *, *, #13707, .T. ) ;
#399 = ORIENTED_EDGE ( 'NONE', *, *, #5094, .F. ) ;
#400 = CARTESIAN_POINT ( 'NONE',  ( 0.5221537403065015237, 44.16218137147968292, 75.45433879953087342 ) ) ;
#401 = ORIENTED_EDGE ( 'NONE', *, *, #18206, .F. ) ;
#402 = PLANE ( 'NONE',  #6711 ) ;
#403 = PLANE ( 'NONE',  #16543 ) ;
#404 = CARTESIAN_POINT ( 'NONE',  ( 4.097390034816026372, 51.53687999803451447, 76.58963291717793709 ) ) ;
#405 = LINE ( 'NONE', #19960, #8602 ) ;
#406 = CARTESIAN_POINT ( 'NONE',  ( -4.812088799398940075, 42.22067586467031930, 93.81371379782397923 ) ) ;
#407 = CARTESIAN_POINT ( 'NONE',  ( 0.8494352808551174361, 52.96349884688018506, 77.70257284945761000 ) ) ;
#409 = DIRECTION ( 'NONE',  ( -1.540237394707284220E-16, -1.793354297423764243E-16, 1.000000000000000000 ) ) ;
#408 = AXIS2_PLACEMENT_3D ( 'NONE', #16155, #16467, #17952 ) ;
#410 = B_SPLINE_CURVE_WITH_KNOTS ( 'NONE', 3,
 ( #6962, #18253, #13567, #3673, #16771, #11880, #20254, #378, #2191, #5261, #14959, #12091, #2405, #20048 ),
 .UNSPECIFIED., .F., .F.,
 ( 4, 2, 2, 2, 2, 2, 4 ),
 ( 0.000000000000000000, 6.529616093792225636E-05, 0.0001305923218758445127, 0.0001958884828137667691, 0.0002611846437516890254, 0.0003917769656275335382, 0.0005223692875033780509 ),
 .UNSPECIFIED. ) ;
#411 = LINE ( 'NONE', #11708, #690 ) ;
#412 = EDGE_CURVE ( 'NONE', #9111, #1287, #34, .T. ) ;
#413 = CARTESIAN_POINT ( 'NONE',  ( -4.567115856812060670, 47.10047254335474065, 90.80496380123797451 ) ) ;
#414 = VECTOR ( 'NONE', #11198, 1000.000000000000227 ) ;
#415 = ORIENTED_EDGE ( 'NONE', *, *, #3915, .F. ) ;
#416 = EDGE_CURVE ( 'NONE', #16577, #9962, #10597, .T. ) ;
#417 = CARTESIAN_POINT ( 'NONE',  ( 0.5753953112280285609, 52.96564479498633204, 75.97198585835440099 ) ) ;
#418 = EDGE_CURVE ( 'NONE', #11233, #17827, #3724, .T. ) ;
#419 = CARTESIAN_POINT ( 'NONE',  ( -4.537713647263719174, 36.95928698179384497, 76.12832907849806929 ) ) ;
#420 = CARTESIAN_POINT ( 'NONE',  ( 33.61275266354798674, 51.36218137147967866, 93.55433879953098142 ) ) ;
#421 = CARTESIAN_POINT ( 'NONE',  ( 8.525177894392134803, 42.37332589716783104, 75.47260332232873736 ) ) ;
#422 = CARTESIAN_POINT ( 'NONE',  ( -2.416137431568557314, 39.07291177436112406, 95.02371380123797451 ) ) ;
#423 = AXIS2_PLACEMENT_3D ( 'NONE', #309, #5407, #15115 ) ;
#424 = CARTESIAN_POINT ( 'NONE',  ( 8.330547866859147277, 41.68096061825437459, 77.50814924735175282 ) ) ;
#425 = PLANE ( 'NONE',  #423 ) ;
#426 = EDGE_CURVE ( 'NONE', #5140, #16560, #15574, .T. ) ;
#427 = VECTOR ( 'NONE', #13805, 1000.000000000000000 ) ;
#428 = CARTESIAN_POINT ( 'NONE',  ( -4.677846259693495767, 44.16218127507053737, 93.01911326394946400 ) ) ;
#429 = ORIENTED_EDGE ( 'NONE', *, *, #5185, .F. ) ;
#430 = EDGE_LOOP ( 'NONE', ( #13284, #4279, #4498, #11595 ) ) ;
#431 = CARTESIAN_POINT ( 'NONE',  ( 8.440918477302592038, 42.45611071105919621, 79.41516958226422673 ) ) ;
#432 = DIRECTION ( 'NONE',  ( 1.402518428993831676E-16, -1.000000000000000000, 0.000000000000000000 ) ) ;
#433 = CARTESIAN_POINT ( 'NONE',  ( 5.543237494533933329, 50.64513746126347371, 78.20513402937135083 ) ) ;
#434 = EDGE_LOOP ( 'NONE', ( #14163, #9298, #3077, #16289 ) ) ;
#435 = APPLICATION_CONTEXT ( 'automotive_design' ) ;
#436 = CARTESIAN_POINT ( 'NONE',  ( -4.534306790193148196, 41.70530359416909505, 95.05433879953095300 ) ) ;
#437 = LINE ( 'NONE', #10027, #19359 ) ;
#438 = CARTESIAN_POINT ( 'NONE',  ( -2.904223097202481174, 48.62752260303690122, 94.08621380294496817 ) ) ;
#439 = CARTESIAN_POINT ( 'NONE',  ( 2.056690051755801996, 52.94072599914807853, 77.29915700192239569 ) ) ;
#440 = CIRCLE ( 'NONE', #3509, 8.199999999999995737 ) ;
#441 = CARTESIAN_POINT ( 'NONE',  ( 3.460444912181559474, 49.25145096859824889, 90.64871380123798872 ) ) ;
#442 = CARTESIAN_POINT ( 'NONE',  ( 8.539681987266121155, 42.43459204878987379, 79.42333176336475731 ) ) ;
#443 = EDGE_LOOP ( 'NONE', ( #16367, #7411, #15591, #11511, #1746, #13003, #15423, #20043, #7490, #3969, #11002, #891 ) ) ;
#444 = DIRECTION ( 'NONE',  ( 0.9534635866061470511, 0.3015081906286169455, 2.009271279954808648E-16 ) ) ;
#445 = VERTEX_POINT ( 'NONE', #20231 ) ;
#446 = DIRECTION ( 'NONE',  ( -0.5954989751681698529, 0.8033560671169786005, 5.234922652618075161E-17 ) ) ;
#447 = CARTESIAN_POINT ( 'NONE',  ( 1.352400422481993658, 50.46853102219002096, 93.07058880123798872 ) ) ;
#448 = ORIENTED_EDGE ( 'NONE', *, *, #4183, .T. ) ;
#449 = CARTESIAN_POINT ( 'NONE',  ( 5.358597061094674707, 45.49318455795749117, 92.47037068152910422 ) ) ;
#450 = VECTOR ( 'NONE', #6055, 1000.000000000000000 ) ;
#451 = CARTESIAN_POINT ( 'NONE',  ( 0.5221537403065064087, 48.16218137147969003, 50.55433879953100273 ) ) ;
#452 = PLANE ( 'NONE',  #15616 ) ;
#453 = ORIENTED_EDGE ( 'NONE', *, *, #3759, .T. ) ;
#454 = FACE_OUTER_BOUND ( 'NONE', #13979, .T. ) ;
#455 = B_SPLINE_CURVE_WITH_KNOTS ( 'NONE', 3,
 ( #16101, #17580, #17484, #9513, #3116, #5991, #4384, #1315, #7797, #14283, #20761, #6195, #8008, #12697, #6292, #11214, #6396, #27, #2128 ),
 .UNSPECIFIED., .F., .F.,
 ( 4, 1, 1, 1, 1, 1, 1, 1, 1, 1, 1, 1, 1, 1, 1, 1, 4 ),
 ( 0.000000000000000000, 0.07819787255609964016, 0.1515336364311310191, 0.2187066978088008651, 0.2814522326392254747, 0.3385163222030129759, 0.3915958516965070690, 0.4406923075239814191, 0.4864642379862412769, 0.5323932679607442653, 0.5831133966729620255, 0.6391356099194271945, 0.6992555458516984679, 0.7657124642625251498, 0.8379597225178306852, 0.9162365097749198828, 1.000000000000000000 ),
 .UNSPECIFIED. ) ;
#456 = EDGE_LOOP ( 'NONE', ( #20112, #3738, #18199, #18118 ) ) ;
#457 = CARTESIAN_POINT ( 'NONE',  ( -3.377490115303421359, 48.14432429247111145, 95.05433879953098142 ) ) ;
#458 = CARTESIAN_POINT ( 'NONE',  ( -7.575063113447651375, 40.56471555772565551, 77.37311125041073012 ) ) ;
#459 = PLANE ( 'NONE',  #12233 ) ;
#460 = CARTESIAN_POINT ( 'NONE',  ( 7.860711257786343609, 47.82081138319720282, 79.44551527011911674 ) ) ;
#461 = CARTESIAN_POINT ( 'NONE',  ( -4.622577041588897373, 46.56120873422322859, 93.81371379782397923 ) ) ;
#462 = CARTESIAN_POINT ( 'NONE',  ( 2.122153740306511160, 47.82824192744436687, 61.55433879953100273 ) ) ;
#463 =( BOUNDED_CURVE ( )  B_SPLINE_CURVE ( 2, ( #19418, #4838, #6543, #14426, #13049, #9754, #20896, #8256, #17929, #12349, #4236, #4725, #16239, #11144, #19523, #4938, #6229 ),
 .UNSPECIFIED., .F., .F. ) 
 B_SPLINE_CURVE_WITH_KNOTS ( ( 3, 2, 2, 2, 2, 2, 2, 2, 3 ),
 ( 0.3050439912557053046, 0.3124899056634827810, 0.3385307311354293081, 0.3645715566073758906, 0.3906123820793224732, 0.4166532075512690003, 0.4426940330232155274, 0.4687348584951621655, 0.4934532648742180339 ),
 .UNSPECIFIED. ) 
 CURVE ( )  GEOMETRIC_REPRESENTATION_ITEM ( )  RATIONAL_B_SPLINE_CURVE ( ( 0.9689162008635190393, 0.9782346958927412572, 1.000000000000000000, 0.9238795325112867385, 1.000000000000000000, 0.9238795325112867385, 1.000000000000000000, 0.9238795325112867385, 1.000000000000000000, 0.9238795325112867385, 1.000000000000000000, 0.9238795325112867385, 1.000000000000000000, 0.9238795325112867385, 1.000000000000000000, 0.9277451227044731796, 0.9926614285408876803 ) ) 
 REPRESENTATION_ITEM ( '' )  );
#464 = VECTOR ( 'NONE', #17169, 1000.000000000000114 ) ;
#465 = EDGE_LOOP ( 'NONE', ( #9711, #3894, #10452, #803 ) ) ;
#466 = CARTESIAN_POINT ( 'NONE',  ( 1.362138928955740402, 52.20745519782975919, 79.45495304649941204 ) ) ;
#467 = CARTESIAN_POINT ( 'NONE',  ( 5.472849728943090852, 37.64179392051541839, 78.35708441643889444 ) ) ;
#468 = VERTEX_POINT ( 'NONE', #12173 ) ;
#469 = CARTESIAN_POINT ( 'NONE',  ( 8.121917471046002035, 44.10225444150351137, 72.45433879953087342 ) ) ;
#470 = ADVANCED_FACE ( 'NONE', ( #18651 ), #4070, .F. ) ;
#471 = CARTESIAN_POINT ( 'NONE',  ( -0.8237052942265477018, 49.18499566818285018, 94.94558879953099506 ) ) ;
#472 = CARTESIAN_POINT ( 'NONE',  ( -2.077846259693550746, 39.65884927180063357, 92.91433879953098085 ) ) ;
#473 = ORIENTED_EDGE ( 'NONE', *, *, #4186, .T. ) ;
#474 = CARTESIAN_POINT ( 'NONE',  ( 2.115041367457929589, 52.20598078514408513, 78.16610350541323271 ) ) ;
#475 = CARTESIAN_POINT ( 'NONE',  ( -5.493714318389452345, 37.66544616749837360, 75.52011153330033721 ) ) ;
#476 = VERTEX_POINT ( 'NONE', #12285 ) ;
#477 = CARTESIAN_POINT ( 'NONE',  ( 5.628424039023946612, 51.33079979992434261, 78.86786983087660019 ) ) ;
#478 = CARTESIAN_POINT ( 'NONE',  ( 0.3727252375183737754, 52.96094423127976825, 77.03975889764973317 ) ) ;
#479 = CARTESIAN_POINT ( 'NONE',  ( 1.868012774839550749, 39.13936707477651566, 91.82058879953099506 ) ) ;
#480 = ORIENTED_EDGE ( 'NONE', *, *, #1486, .F. ) ;
#481 = CARTESIAN_POINT ( 'NONE',  ( -4.147711664773192197, 37.44596934634147800, 78.25995115514949418 ) ) ;
#482 = CARTESIAN_POINT ( 'NONE',  ( 1.352400422481993658, 50.46853102219002096, 95.72683880123798872 ) ) ;
#483 = ORIENTED_EDGE ( 'NONE', *, *, #9901, .T. ) ;
#484 = CARTESIAN_POINT ( 'NONE',  ( -3.677846259693500652, 44.16218137147969003, 45.55433879953098852 ) ) ;
#485 = CARTESIAN_POINT ( 'NONE',  ( 9.353817388681445522, 42.82770861117572281, 78.41904468188381827 ) ) ;
#486 = DIRECTION ( 'NONE',  ( 0.000000000000000000, 0.000000000000000000, 1.000000000000000000 ) ) ;
#487 = EDGE_CURVE ( 'NONE', #10540, #2739, #17166, .T. ) ;
#488 = CARTESIAN_POINT ( 'NONE',  ( 6.591015671753180705, 50.61977213638343187, 75.57514290624801845 ) ) ;
#489 = CARTESIAN_POINT ( 'NONE',  ( 5.581406744796363562, 50.61539444998253856, 76.90580938776616904 ) ) ;
#490 = CARTESIAN_POINT ( 'NONE',  ( -2.917199766949189588, 51.60602765227618960, 72.45433879953087342 ) ) ;
#491 = ORIENTED_EDGE ( 'NONE', *, *, #20174, .T. ) ;
#492 = VERTEX_POINT ( 'NONE', #14650 ) ;
#493 = CARTESIAN_POINT ( 'NONE',  ( 11.22215374030650281, 42.76218137147968434, 61.40715055817103263 ) ) ;
#494 = EDGE_CURVE ( 'NONE', #20602, #3211, #14857, .T. ) ;
#495 = CARTESIAN_POINT ( 'NONE',  ( 7.847142571091401564, 40.67652665170315629, 79.34450935619591405 ) ) ;
#496 = VERTEX_POINT ( 'NONE', #21015 ) ;
#497 = DIRECTION ( 'NONE',  ( 0.4999999999999984457, 0.8660254037844394848, -0.000000000000000000 ) ) ;
#498 = DIRECTION ( 'NONE',  ( 0.3165065846431717178, 0.9485903129789564625, 0.000000000000000000 ) ) ;
#499 = CARTESIAN_POINT ( 'NONE',  ( -5.154188915835984375, 42.64120994080404614, 94.86746380123797451 ) ) ;
#500 = VERTEX_POINT ( 'NONE', #77 ) ;
#501 = PLANE ( 'NONE',  #17443 ) ;
#502 = VERTEX_POINT ( 'NONE', #9881 ) ;
#503 = CARTESIAN_POINT ( 'NONE',  ( -3.495367959724245299, 36.18934821065389684, 76.68008248600652621 ) ) ;
#504 = FACE_OUTER_BOUND ( 'NONE', #17510, .T. ) ;
#505 = CARTESIAN_POINT ( 'NONE',  ( -3.382808528096845180, 51.37448915066374155, 79.35174982259798071 ) ) ;
#506 = CARTESIAN_POINT ( 'NONE',  ( 8.378637954445377289, 41.81363803720061867, 77.14698585835439815 ) ) ;
#507 = CARTESIAN_POINT ( 'NONE',  ( 0.5221537403065005245, 44.16218137147968292, 82.45433879953087342 ) ) ;
#508 = CARTESIAN_POINT ( 'NONE',  ( 8.862035351310685982, 41.35380664710483245, 75.97281361087948426 ) ) ;
#509 = CARTESIAN_POINT ( 'NONE',  ( 2.563360104887116631, 38.63792983641089052, 92.55433879953098142 ) ) ;
#510 = DIRECTION ( 'NONE',  ( 1.000000000000000000, 0.000000000000000000, 1.196361017915039239E-16 ) ) ;
#511 = CARTESIAN_POINT ( 'NONE',  ( 5.210818179720607013, 37.44367253161215103, 77.75193993234761081 ) ) ;
#512 = CARTESIAN_POINT ( 'NONE',  ( 6.198496396448986090, 45.68315280215533392, 91.58621380123798872 ) ) ;
#513 = CARTESIAN_POINT ( 'NONE',  ( 0.5221537403065010796, 44.16218137147969003, 54.55433879953099563 ) ) ;
#514 = CARTESIAN_POINT ( 'NONE',  ( 0.3418901990080560060, 52.35614732999829357, 76.10778090364108550 ) ) ;
#515 = ORIENTED_EDGE ( 'NONE', *, *, #17085, .T. ) ;
#516 = CARTESIAN_POINT ( 'NONE',  ( 27.03948732994508930, 43.16218137147969003, 76.90433879953101837 ) ) ;
#517 = CARTESIAN_POINT ( 'NONE',  ( -1.477846259693498476, 49.81903562097206617, 67.21119304902336467 ) ) ;
#518 = CARTESIAN_POINT ( 'NONE',  ( -4.513346507200660440, 37.69592389900041240, 78.81125587425833601 ) ) ;
#519 = CARTESIAN_POINT ( 'NONE',  ( 5.611423337425062385, 41.22389019960463230, 94.08621380123797451 ) ) ;
#520 = EDGE_CURVE ( 'NONE', #7726, #2743, #10893, .T. ) ;
#521 = CARTESIAN_POINT ( 'NONE',  ( -4.895593109503407092, 37.22363812428621088, 76.38448585835440952 ) ) ;
#522 = FACE_OUTER_BOUND ( 'NONE', #11678, .T. ) ;
#523 = EDGE_CURVE ( 'NONE', #18140, #20811, #17951, .T. ) ;
#524 = CARTESIAN_POINT ( 'NONE',  ( 5.388356174074294458, 50.75501278463794819, 77.94845644658968808 ) ) ;
#525 = ORIENTED_EDGE ( 'NONE', *, *, #8421, .T. ) ;
#526 = ORIENTED_EDGE ( 'NONE', *, *, #20016, .T. ) ;
#527 = CARTESIAN_POINT ( 'NONE',  ( 6.521540251228659990, 49.75211551535583965, 76.74525360924829442 ) ) ;
#528 = CARTESIAN_POINT ( 'NONE',  ( 28.52215374030649642, 44.16218137147969003, 105.5543387995310098 ) ) ;
#529 = EDGE_CURVE ( 'NONE', #6977, #4812, #7370, .T. ) ;
#530 = CARTESIAN_POINT ( 'NONE',  ( 5.542822135681054085, 50.64549836037226527, 78.13134938951201036 ) ) ;
#531 = VERTEX_POINT ( 'NONE', #5064 ) ;
#532 = CARTESIAN_POINT ( 'NONE',  ( 0.3679909894256196412, 52.36076605197753508, 77.03976057311564318 ) ) ;
#533 = DIRECTION ( 'NONE',  ( 3.893792155548169402E-16, 7.183611964723547524E-17, -1.000000000000000000 ) ) ;
#534 = EDGE_CURVE ( 'NONE', #17146, #7324, #19941, .T. ) ;
#535 = CARTESIAN_POINT ( 'NONE',  ( -1.077846259693481024, 50.16218137147969713, 69.55433879953100984 ) ) ;
#536 = CARTESIAN_POINT ( 'NONE',  ( -0.8237052942265477018, 49.18499566818285018, 92.75808880294498238 ) ) ;
#537 = CARTESIAN_POINT ( 'NONE',  ( -7.804011829531284583, 41.29348983807560813, 78.85792113001433279 ) ) ;
#538 = CARTESIAN_POINT ( 'NONE',  ( -2.416137431568557314, 39.07291177436112406, 92.36746380123797451 ) ) ;
#539 = CARTESIAN_POINT ( 'NONE',  ( 4.394343283833276992, 39.11584570990505938, 91.50808880123798872 ) ) ;
#540 = PRODUCT ( 'Washer', 'Washer', '', ( #5689 ) ) ;
#541 = CARTESIAN_POINT ( 'NONE',  ( -3.245259920192584691, 36.91861848204638363, 77.89282216559597316 ) ) ;
#542 = CARTESIAN_POINT ( 'NONE',  ( -7.938266955593502594, 41.73948448446050463, 79.54486073715324324 ) ) ;
#543 = ORIENTED_EDGE ( 'NONE', *, *, #8222, .F. ) ;
#544 = CARTESIAN_POINT ( 'NONE',  ( 0.8503282811412342657, 52.95606000782371581, 72.45433879953087342 ) ) ;
#545 = EDGE_LOOP ( 'NONE', ( #1618, #377, #11663, #17754 ) ) ;
#546 = CARTESIAN_POINT ( 'NONE',  ( 3.357643116058060428, 50.56218137147968861, 95.05433879953096721 ) ) ;
#547 = CARTESIAN_POINT ( 'NONE',  ( 2.043125170982144745, 38.48583871533720213, 92.52371380123798872 ) ) ;
#548 = ORIENTED_EDGE ( 'NONE', *, *, #4583, .T. ) ;
#549 = DIRECTION ( 'NONE',  ( -5.626130192357176673E-16, -1.831515347669941892E-30, 1.000000000000000000 ) ) ;
#550 = DIRECTION ( 'NONE',  ( -0.5773502691896219563, 0.5773502691896226224, -0.5773502691896327255 ) ) ;
#551 = VECTOR ( 'NONE', #6158, 1000.000000000000000 ) ;
#552 = CARTESIAN_POINT ( 'NONE',  ( -3.477340361660131496, 52.12006153457090818, 79.00686454089694166 ) ) ;
#553 = DIRECTION ( 'NONE',  ( 0.9429220365244146418, -0.3330135628418914862, 8.551124769255465366E-17 ) ) ;
#554 = DIRECTION ( 'NONE',  ( 3.893792155548169402E-16, 7.183611964723547524E-17, -1.000000000000000000 ) ) ;
#555 = EDGE_CURVE ( 'NONE', #18406, #13226, #12465, .T. ) ;
#556 = CARTESIAN_POINT ( 'NONE',  ( 3.117507734380599693, 51.94062193790708903, 72.45433879953087342 ) ) ;
#557 = VERTEX_POINT ( 'NONE', #590 ) ;
#558 = CARTESIAN_POINT ( 'NONE',  ( 8.378637954445377289, 41.81363803720061867, 77.14698585835439815 ) ) ;
#559 = VERTEX_POINT ( 'NONE', #18472 ) ;
#560 = DIRECTION ( 'NONE',  ( -0.000000000000000000, -0.000000000000000000, 1.000000000000000000 ) ) ;
#561 = DIRECTION ( 'NONE',  ( -0.9999689119394086223, 0.007885122365275665235, -1.526048693634353392E-16 ) ) ;
#562 = CARTESIAN_POINT ( 'NONE',  ( -8.192078482032012943, 42.93655631659661509, 78.13669174070733447 ) ) ;
#563 = FACE_OUTER_BOUND ( 'NONE', #14057, .T. ) ;
#564 = CARTESIAN_POINT ( 'NONE',  ( 5.666884522201894647, 41.76315400873614436, 94.28246379782397923 ) ) ;
#565 = CARTESIAN_POINT ( 'NONE',  ( 5.492130682024771282, 37.64468814625064397, 76.33129752952908120 ) ) ;
#566 = CIRCLE ( 'NONE', #9426, 6.000000000000002665 ) ;
#567 = ORIENTED_EDGE ( 'NONE', *, *, #9336, .T. ) ;
#568 = CARTESIAN_POINT ( 'NONE',  ( 8.213883505808539098, 41.33151258250490656, 78.76104738055306598 ) ) ;
#569 = ORIENTED_EDGE ( 'NONE', *, *, #6995, .T. ) ;
#570 = CARTESIAN_POINT ( 'NONE',  ( 10.77494014480653561, 42.96218137147968008, 65.80574467885102763 ) ) ;
#571 = CARTESIAN_POINT ( 'NONE',  ( 5.544968037009670780, 45.50804040601273925, 95.88308879953100927 ) ) ;
#572 = CARTESIAN_POINT ( 'NONE',  ( 6.102441102155617969, 43.42752260303680600, 95.80496379953099506 ) ) ;
#573 = CARTESIAN_POINT ( 'NONE',  ( -7.163641313832624036, 41.71182641517503953, 77.97272179757899835 ) ) ;
#574 = ORIENTED_EDGE ( 'NONE', *, *, #4534, .T. ) ;
#575 = CARTESIAN_POINT ( 'NONE',  ( 11.22215374030650281, 42.76218137147968434, 57.80715055817105252 ) ) ;
#576 = CARTESIAN_POINT ( 'NONE',  ( 0.5221537403065006355, 44.16218137147969003, 92.45433879953097289 ) ) ;
#577 = ORIENTED_EDGE ( 'NONE', *, *, #17193, .T. ) ;
#578 = CARTESIAN_POINT ( 'NONE',  ( 1.864804668130312537, 39.18816951145882399, 95.05433879953096721 ) ) ;
#579 = CARTESIAN_POINT ( 'NONE',  ( -4.790699304645749557, 51.18158331905331693, 78.75763390087725213 ) ) ;
#580 = CARTESIAN_POINT ( 'NONE',  ( -2.077846259693550746, 39.65884927180063357, 91.66433879953099506 ) ) ;
#581 = ORIENTED_EDGE ( 'NONE', *, *, #5982, .F. ) ;
#582 = CARTESIAN_POINT ( 'NONE',  ( 2.115041367457929589, 52.20598078514408513, 78.16610350541323271 ) ) ;
#583 = CARTESIAN_POINT ( 'NONE',  ( 5.544968037009670780, 45.50804040601273925, 90.88308879953099506 ) ) ;
#584 = CIRCLE ( 'NONE', #4658, 3.999999999999996447 ) ;
#585 = VERTEX_POINT ( 'NONE', #7187 ) ;
#586 = CARTESIAN_POINT ( 'NONE',  ( -4.804516487068378083, 51.17171006637344277, 76.41659450085566618 ) ) ;
#587 = CARTESIAN_POINT ( 'NONE',  ( 0.5221537403065005245, 44.16218137147968292, 82.45433879953087342 ) ) ;
#588 =( BOUNDED_SURFACE ( )  B_SPLINE_SURFACE ( 1, 2, ( 
 ( #3661, #10172, #3971, #17175, #10717, #11978, #8994, #15159, #12183, #2503, #571, #8571, #13770, #15058, #8892, #19926, #5354, #4081, #2279, #20142, #2391, #10391, #471, #3869, #15482, #10497, #5574, #10608, #12078, #7054, #13554, #20032, #18454, #18344, #3763, #13454, #16961, #6949, #10282, #11867, #18558, #15268, #15380, #794, #7278, #16759, #20242, #688, #2179, #5791, #893, #5673, #8679, #18661, #17077, #5464, #16860, #7167, #7381, #8778, #13871, #13667, #20352, #12296, #18776, #4191, #19088, #9097, #16001, #7803, #12490, #13984, #14181, #11016, #5996, #6296, #17487, #20466, #20765 ),
 ( #5901, #15801, #1214, #18977, #6199, #14397, #14289, #12398, #1422, #20569, #9208, #18877, #11220, #2601, #2913, #7907, #1000, #20866, #15585, #7494, #4388, #10914, #9315, #17383, #4284, #15695, #9518, #12797, #1114, #7703, #7603, #11116, #12701, #2810, #4694, #19280, #9411, #10811, #20660, #19178, #17277, #3012, #2701, #6094, #14086, #12599, #4496, #15899, #1319, #4592, #17584, #13016, #6609, #19490, #8330, #2233, #14710, #17798, #16314, #19388, #5528, #13116, #16425, #20965, #16206, #8011, #132, #3222, #31, #16816, #6509, #14605, #5119, #8115, #19700, #3321, #14497, #6400, #3537 ) ),
 .UNSPECIFIED., .F., .F., .T. ) 
 B_SPLINE_SURFACE_WITH_KNOTS ( ( 2, 2 ),
 ( 3, 2, 2, 2, 2, 2, 2, 2, 2, 2, 2, 2, 2, 2, 2, 2, 2, 2, 2, 2, 2, 2, 2, 2, 2, 2, 2, 2, 2, 2, 2, 2, 2, 2, 2, 2, 2, 2, 2, 3 ),
 ( 0.000000000000000000, 1.000000000000000000 ),
 ( 0.000000000000000000, 0.02500000000000000139, 0.05000000000000000278, 0.07499999999999999722, 0.1000000000000000056, 0.1250000000000000000, 0.1499999999999999944, 0.1749999999999999889, 0.2000000000000000111, 0.2250000000000000056, 0.2500000000000000000, 0.2750000000000000222, 0.2999999999999999889, 0.3250000000000000111, 0.3499999999999999778, 0.3750000000000000000, 0.4000000000000000222, 0.4249999999999999889, 0.4500000000000000111, 0.4749999999999999778, 0.5000000000000000000, 0.5250000000000000222, 0.5500000000000000444, 0.5749999999999999556, 0.5999999999999999778, 0.6250000000000000000, 0.6500000000000000222, 0.6750000000000000444, 0.6999999999999999556, 0.7249999999999999778, 0.7500000000000000000, 0.7750000000000000222, 0.8000000000000000444, 0.8249999999999999556, 0.8499999999999999778, 0.8750000000000000000, 0.9000000000000000222, 0.9250000000000000444, 0.9499999999999999556, 0.9600310108036838042 ),
 .UNSPECIFIED. ) 
 GEOMETRIC_REPRESENTATION_ITEM ( )  RATIONAL_B_SPLINE_SURFACE ( (
 ( 1.000000000000000000, 0.9238795325112867385, 1.000000000000000000, 0.9238795325112867385, 1.000000000000000000, 0.9238795325112867385, 1.000000000000000000, 0.9238795325112867385, 1.000000000000000000, 0.9238795325112867385, 1.000000000000000000, 0.9238795325112867385, 1.000000000000000000, 0.9238795325112867385, 1.000000000000000000, 0.9238795325112867385, 1.000000000000000000, 0.9238795325112867385, 1.000000000000000000, 0.9238795325112867385, 1.000000000000000000, 0.9238795325112867385, 1.000000000000000000, 0.9238795325112867385, 1.000000000000000000, 0.9238795325112867385, 1.000000000000000000, 0.9238795325112867385, 1.000000000000000000, 0.9238795325112867385, 1.000000000000000000, 0.9238795325112867385, 1.000000000000000000, 0.9238795325112867385, 1.000000000000000000, 0.9238795325112867385, 1.000000000000000000, 0.9238795325112867385, 1.000000000000000000, 0.9238795325112867385, 1.000000000000000000, 0.9238795325112867385, 1.000000000000000000, 0.9238795325112867385, 1.000000000000000000, 0.9238795325112867385, 1.000000000000000000, 0.9238795325112867385, 1.000000000000000000, 0.9238795325112867385, 1.000000000000000000, 0.9238795325112867385, 1.000000000000000000, 0.9238795325112867385, 1.000000000000000000, 0.9238795325112867385, 1.000000000000000000, 0.9238795325112867385, 1.000000000000000000, 0.9238795325112867385, 1.000000000000000000, 0.9238795325112867385, 1.000000000000000000, 0.9238795325112867385, 1.000000000000000000, 0.9238795325112867385, 1.000000000000000000, 0.9238795325112867385, 1.000000000000000000, 0.9238795325112867385, 1.000000000000000000, 0.9238795325112867385, 1.000000000000000000, 0.9238795325112867385, 1.000000000000000000, 0.9238795325112867385, 1.000000000000000000, 0.9694573907295700455, 0.9634246409442903669),
 ( 1.000000000000000000, 0.9238795325112867385, 1.000000000000000000, 0.9238795325112867385, 1.000000000000000000, 0.9238795325112867385, 1.000000000000000000, 0.9238795325112867385, 1.000000000000000000, 0.9238795325112867385, 1.000000000000000000, 0.9238795325112867385, 1.000000000000000000, 0.9238795325112867385, 1.000000000000000000, 0.9238795325112867385, 1.000000000000000000, 0.9238795325112867385, 1.000000000000000000, 0.9238795325112867385, 1.000000000000000000, 0.9238795325112867385, 1.000000000000000000, 0.9238795325112867385, 1.000000000000000000, 0.9238795325112867385, 1.000000000000000000, 0.9238795325112867385, 1.000000000000000000, 0.9238795325112867385, 1.000000000000000000, 0.9238795325112867385, 1.000000000000000000, 0.9238795325112867385, 1.000000000000000000, 0.9238795325112867385, 1.000000000000000000, 0.9238795325112867385, 1.000000000000000000, 0.9238795325112867385, 1.000000000000000000, 0.9238795325112867385, 1.000000000000000000, 0.9238795325112867385, 1.000000000000000000, 0.9238795325112867385, 1.000000000000000000, 0.9238795325112867385, 1.000000000000000000, 0.9238795325112867385, 1.000000000000000000, 0.9238795325112867385, 1.000000000000000000, 0.9238795325112867385, 1.000000000000000000, 0.9238795325112867385, 1.000000000000000000, 0.9238795325112867385, 1.000000000000000000, 0.9238795325112867385, 1.000000000000000000, 0.9238795325112867385, 1.000000000000000000, 0.9238795325112867385, 1.000000000000000000, 0.9238795325112867385, 1.000000000000000000, 0.9238795325112867385, 1.000000000000000000, 0.9238795325112867385, 1.000000000000000000, 0.9238795325112867385, 1.000000000000000000, 0.9238795325112867385, 1.000000000000000000, 0.9238795325112867385, 1.000000000000000000, 0.9694573907295700455, 0.9634246409442903669) ) ) 
 REPRESENTATION_ITEM ( '' )  SURFACE ( )  );
#589 = CARTESIAN_POINT ( 'NONE',  ( -3.603146387903923387, 36.26895979397031056, 78.01078865174693533 ) ) ;
#590 = CARTESIAN_POINT ( 'NONE',  ( -4.895593109503407092, 37.22363812428621088, 77.05433879953086773 ) ) ;
#591 = EDGE_CURVE ( 'NONE', #11321, #18929, #15285, .T. ) ;
#592 = VECTOR ( 'NONE', #12454, 1000.000000000000000 ) ;
#593 = DIRECTION ( 'NONE',  ( 0.9999542261909885044, 0.009567942452863074584, 1.557325602890291209E-16 ) ) ;
#594 = ORIENTED_EDGE ( 'NONE', *, *, #1429, .T. ) ;
#595 = CARTESIAN_POINT ( 'NONE',  ( 0.5221537403065015237, 44.16218137147968292, 75.45433879953088763 ) ) ;
#596 = AXIS2_PLACEMENT_3D ( 'NONE', #2312, #15191, #5384 ) ;
#597 = VERTEX_POINT ( 'NONE', #10084 ) ;
#598 = CARTESIAN_POINT ( 'NONE',  ( -4.982544207447554108, 38.08376228894968563, 75.45541555965391467 ) ) ;
#599 = LINE ( 'NONE', #15297, #5135 ) ;
#600 = LINE ( 'NONE', #11898, #16389 ) ;
#601 = CARTESIAN_POINT ( 'NONE',  ( -3.358136819263964234, 52.20524002164697208, 76.41354228756682687 ) ) ;
#602 = ORIENTED_EDGE ( 'NONE', *, *, #4967, .F. ) ;
#603 = EDGE_CURVE ( 'NONE', #17868, #14152, #6557, .T. ) ;
#604 = LINE ( 'NONE', #5382, #12018 ) ;
#605 = ORIENTED_EDGE ( 'NONE', *, *, #8324, .F. ) ;
#606 = CARTESIAN_POINT ( 'NONE',  ( 4.577225057937401864, 52.10727814237509392, 78.46169174070733732 ) ) ;
#607 = CARTESIAN_POINT ( 'NONE',  ( 5.833402057135029573, 38.06140832622005377, 75.44618574453703275 ) ) ;
#608 = VECTOR ( 'NONE', #1076, 1000.000000000000000 ) ;
#609 = CARTESIAN_POINT ( 'NONE',  ( 9.204112107805267229, 42.37903238726386945, 75.57016332177543916 ) ) ;
#610 = CARTESIAN_POINT ( 'NONE',  ( 4.605781907348109883, 52.08618434805546116, 77.30394856433355244 ) ) ;
#611 = CARTESIAN_POINT ( 'NONE',  ( 27.03948732994508930, 36.35905713404685713, 76.90433879953101837 ) ) ;
#612 = DIRECTION ( 'NONE',  ( -1.000000000000000000, -1.402518428993831676E-16, -1.196361017915039239E-16 ) ) ;
#613 = CARTESIAN_POINT ( 'NONE',  ( 0.6761804647047966466, 52.35351123918825067, 77.39848739855237625 ) ) ;
#614 = CARTESIAN_POINT ( 'NONE',  ( 2.522153740306493308, 49.81903562097208749, 59.21119304902340019 ) ) ;
#615 = CARTESIAN_POINT ( 'NONE',  ( 5.939900590116411472, 51.10072461867315496, 76.90580938776616904 ) ) ;
#616 = CARTESIAN_POINT ( 'NONE',  ( 1.352400422481993658, 50.46853102219002096, 93.07058880123798872 ) ) ;
#617 = DIRECTION ( 'NONE',  ( -0.9209602848141236198, 0.007262110304243513635, 0.3895887774936765968 ) ) ;
#618 = VERTEX_POINT ( 'NONE', #18367 ) ;
#619 = CARTESIAN_POINT ( 'NONE',  ( 0.3790988156517668406, 52.35585392638166979, 76.04467822456393833 ) ) ;
#620 = CIRCLE ( 'NONE', #2330, 6.999999999999999112 ) ;
#621 = ORIENTED_EDGE ( 'NONE', *, *, #3762, .F. ) ;
#622 = CARTESIAN_POINT ( 'NONE',  ( 5.203405869548749507, 50.89463106707474083, 76.94936699987064799 ) ) ;
#623 = DIRECTION ( 'NONE',  ( 5.595882180570345180E-16, -1.000000000000000000, 6.798436021654163964E-32 ) ) ;
#624 = PRODUCT_RELATED_PRODUCT_CATEGORY ( 'part', '', ( #3765 ) ) ;
#625 = CARTESIAN_POINT ( 'NONE',  ( -3.405315259844419185, 52.17152803532113126, 78.78030711080756987 ) ) ;
#626 = CARTESIAN_POINT ( 'NONE',  ( -4.567115856812060670, 47.10047254335474065, 95.96121380123798872 ) ) ;
#627 = DIRECTION ( 'NONE',  ( -1.000000000000000000, 0.000000000000000000, 0.000000000000000000 ) ) ;
#628 = CARTESIAN_POINT ( 'NONE',  ( -7.450195187915191752, 48.08726987376739714, 78.78375056423675460 ) ) ;
#629 = CARTESIAN_POINT ( 'NONE',  ( 11.22215374030650281, 42.96218137147968008, 69.40574467885102194 ) ) ;
#630 = EDGE_CURVE ( 'NONE', #9317, #1035, #3784, .T. ) ;
#631 = PLANE ( 'NONE',  #10880 ) ;
#632 = ORIENTED_EDGE ( 'NONE', *, *, #10851, .F. ) ;
#633 = ORIENTED_EDGE ( 'NONE', *, *, #11977, .T. ) ;
#634 = EDGE_CURVE ( 'NONE', #18929, #10043, #16879, .T. ) ;
#635 = CARTESIAN_POINT ( 'NONE',  ( 6.446408651871711193, 49.83176319091943896, 77.36971804863098612 ) ) ;
#636 = DIRECTION ( 'NONE',  ( 0.9485903129789527988, -0.3165065846431829311, 8.934458285744989980E-17 ) ) ;
#637 = LINE ( 'NONE', #18411, #13677 ) ;
#638 = ORIENTED_EDGE ( 'NONE', *, *, #15893, .T. ) ;
#639 = CARTESIAN_POINT ( 'NONE',  ( -5.510796958474740492, 38.60848837797752964, 78.18375056423674607 ) ) ;
#640 = CARTESIAN_POINT ( 'NONE',  ( -1.219056181836355446, 49.77488197367695477, 93.15612966814926210 ) ) ;
#641 = CIRCLE ( 'NONE', #12556, 8.199999999999995737 ) ;
#642 = CARTESIAN_POINT ( 'NONE',  ( 28.52215374030649642, 40.16218137147968292, 87.85433879953103542 ) ) ;
#643 = CARTESIAN_POINT ( 'NONE',  ( -5.058133621542618030, 44.89684013992257405, 90.49246380294498238 ) ) ;
#644 = ADVANCED_FACE ( 'NONE', ( #384 ), #18159, .T. ) ;
#645 = CARTESIAN_POINT ( 'NONE',  ( 2.118841533926105303, 52.94023591187011846, 77.68224048311739693 ) ) ;
#646 = CARTESIAN_POINT ( 'NONE',  ( -3.625666805699584216, 36.28559471941820647, 77.96849812480175501 ) ) ;
#647 = EDGE_CURVE ( 'NONE', #15434, #225, #16566, .T. ) ;
#648 = CARTESIAN_POINT ( 'NONE',  ( 3.460444912181559474, 49.25145096859824889, 92.99246380123798872 ) ) ;
#649 = PRODUCT_RELATED_PRODUCT_CATEGORY ( 'part', '', ( #18386 ) ) ;
#650 = CARTESIAN_POINT ( 'NONE',  ( -8.174140996651441782, 42.81404400550773914, 78.99660062231663460 ) ) ;
#651 = ORIENTED_EDGE ( 'NONE', *, *, #14253, .F. ) ;
#652 = EDGE_CURVE ( 'NONE', #1084, #8801, #11683, .T. ) ;
#653 = DIRECTION ( 'NONE',  ( 1.110223024625156540E-16, 1.000000000000000000, 5.922860397471808077E-17 ) ) ;
#654 = EDGE_CURVE ( 'NONE', #7531, #3376, #7648, .T. ) ;
#655 = VECTOR ( 'NONE', #8630, 1000.000000000000114 ) ;
#656 = EDGE_LOOP ( 'NONE', ( #3980, #17099, #14768, #7284, #18986, #9998 ) ) ;
#657 = CARTESIAN_POINT ( 'NONE',  ( -4.352345764855491517, 50.74789927721977989, 78.91934866582661812 ) ) ;
#658 = CARTESIAN_POINT ( 'NONE',  ( 4.987494971863720927, 47.58855820898865829, 95.02371380294496817 ) ) ;
#659 = ORIENTED_EDGE ( 'NONE', *, *, #9004, .F. ) ;
#660 = CARTESIAN_POINT ( 'NONE',  ( 8.281609818839775983, 41.50998675140334626, 78.01310313856961898 ) ) ;
#662 = AXIS2_PLACEMENT_3D ( 'NONE', #12850, #6249, #17746 ) ;
#661 = CARTESIAN_POINT ( 'NONE',  ( -4.009385194876762704, 46.27527268018315709, 94.51683879953097289 ) ) ;
#663 = CARTESIAN_POINT ( 'NONE',  ( -4.471346911670678992, 51.40978084683593607, 79.54642512701808243 ) ) ;
#664 = CARTESIAN_POINT ( 'NONE',  ( 0.5221537403064985261, 44.16218137147969003, 96.05433879953096721 ) ) ;
#665 = PLANE ( 'NONE',  #18587 ) ;
#666 = CARTESIAN_POINT ( 'NONE',  ( 0.3279354642496041250, 52.35625728194811046, 78.50066232894263862 ) ) ;
#667 = VERTEX_POINT ( 'NONE', #6965 ) ;
#668 = CARTESIAN_POINT ( 'NONE',  ( 8.271884794240664363, 41.48202034606706690, 77.51897818627048764 ) ) ;
#669 = VECTOR ( 'NONE', #11258, 1000.000000000000000 ) ;
#670 = ORIENTED_EDGE ( 'NONE', *, *, #19379, .F. ) ;
#671 = DIRECTION ( 'NONE',  ( -0.007885122365275663500, -0.9999689119394085113, -1.805443505845543142E-16 ) ) ;
#672 = CARTESIAN_POINT ( 'NONE',  ( 6.931410089129659724, 50.36833649219094866, 77.12327887040382279 ) ) ;
#673 = VECTOR ( 'NONE', #16974, 1000.000000000000000 ) ;
#674 = AXIS2_PLACEMENT_3D ( 'NONE', #3348, #6948, #15057 ) ;
#675 = CARTESIAN_POINT ( 'NONE',  ( 3.460444912181559474, 49.25145096859824889, 93.14871380123798872 ) ) ;
#676 = CARTESIAN_POINT ( 'NONE',  ( 6.554687423727395768, 50.64660634980899090, 79.34836068132329956 ) ) ;
#677 = DIRECTION ( 'NONE',  ( 0.8043570849667761591, -0.5941461771851692664, 1.733862608106489734E-17 ) ) ;
#678 = CARTESIAN_POINT ( 'NONE',  ( 5.666884522201896424, 41.76315400873614436, 91.93871379782397923 ) ) ;
#679 = CARTESIAN_POINT ( 'NONE',  ( -5.728661668566965126, 37.83899231081795023, 75.70067668752250256 ) ) ;
#680 = CONICAL_SURFACE ( 'NONE', #9184, 6.200000000000020606, 1.047197551196600518 ) ;
#681 = VECTOR ( 'NONE', #16748, 1000.000000000000000 ) ;
#682 = VERTEX_POINT ( 'NONE', #13470 ) ;
#683 = ADVANCED_FACE ( 'NONE', ( #20262 ), #4587, .T. ) ;
#684 = CARTESIAN_POINT ( 'NONE',  ( 8.248434610079064200, 41.43506443388486815, 78.91056401563228917 ) ) ;
#685 = B_SPLINE_CURVE_WITH_KNOTS ( 'NONE', 3,
 ( #20191, #622, #6998, #11320, #2227, #14601, #3317, #11922, #10227, #18287 ),
 .UNSPECIFIED., .F., .F.,
 ( 4, 2, 2, 2, 4 ),
 ( 0.000000000000000000, 0.0001306217549985001693, 0.0002612435099970003387, 0.0003918652649955005080, 0.0005224870199940006774 ),
 .UNSPECIFIED. ) ;
#686 = ORIENTED_EDGE ( 'NONE', *, *, #5989, .F. ) ;
#687 = CARTESIAN_POINT ( 'NONE',  ( -4.217603907031332255, 50.67132072554849742, 75.36022115247205022 ) ) ;
#688 = CARTESIAN_POINT ( 'NONE',  ( -0.2125050281363792815, 38.58189400963055959, 92.99246379953098085 ) ) ;
#689 = CARTESIAN_POINT ( 'NONE',  ( -2.077846259693550746, 39.65884927180063357, 94.16433879953098085 ) ) ;
#690 = VECTOR ( 'NONE', #7095, 1000.000000000000000 ) ;
#691 = ORIENTED_EDGE ( 'NONE', *, *, #6268, .F. ) ;
#692 = CARTESIAN_POINT ( 'NONE',  ( -0.3080929418689875576, 37.85583172076933778, 92.60183880123797451 ) ) ;
#693 = DIRECTION ( 'NONE',  ( 0.8136266022444372803, 0.5813877811927012917, 2.295812393977109593E-16 ) ) ;
#694 = CARTESIAN_POINT ( 'NONE',  ( 5.471341376803050771, 36.88291743766401254, 75.36841521003546518 ) ) ;
#695 = CARTESIAN_POINT ( 'NONE',  ( 0.3821786226492926430, 35.36301154328572949, 76.86610350541323555 ) ) ;
#696 = ORIENTED_EDGE ( 'NONE', *, *, #11737, .F. ) ;
#697 = DIRECTION ( 'NONE',  ( 1.334402673828313339E-16, 1.871524341742854397E-32, -1.000000000000000000 ) ) ;
#698 = CARTESIAN_POINT ( 'NONE',  ( -2.416137431568557314, 39.07291177436112406, 95.02371380123797451 ) ) ;
#699 = AXIS2_PLACEMENT_3D ( 'NONE', #10681, #862, #6061 ) ;
#700 = EDGE_LOOP ( 'NONE', ( #2325, #17366, #15726, #14088 ) ) ;
#701 = CARTESIAN_POINT ( 'NONE',  ( -4.450958381679031461, 50.67743431167600932, 76.37148643835737971 ) ) ;
#702 = DIRECTION ( 'NONE',  ( 0.007885122365275663500, 0.9999689119394085113, 1.805443505845543142E-16 ) ) ;
#703 = CARTESIAN_POINT ( 'NONE',  ( 5.568489401881125289, 48.03437091500646261, 91.66433880123796030 ) ) ;
#704 = CONTEXT_DEPENDENT_SHAPE_REPRESENTATION ( #14978, #8714 ) ;
#705 = CARTESIAN_POINT ( 'NONE',  ( -4.534767414998234436, 37.71174666070368175, 76.36316342150684022 ) ) ;
#706 = PRODUCT_DEFINITION_FORMATION_WITH_SPECIFIED_SOURCE ( 'ANY', '', #19896, .NOT_KNOWN. ) ;
#707 = CARTESIAN_POINT ( 'NONE',  ( 0.4269670398180140936, 52.96169137011722228, 78.89164370455331721 ) ) ;
#708 = FACE_OUTER_BOUND ( 'NONE', #9864, .T. ) ;
#709 = ORIENTED_EDGE ( 'NONE', *, *, #18588, .F. ) ;
#710 = CARTESIAN_POINT ( 'NONE',  ( 0.5922593966368500107, 52.21352501355296738, 75.36022115247205022 ) ) ;
#711 = ORIENTED_EDGE ( 'NONE', *, *, #20025, .F. ) ;
#712 = FACE_OUTER_BOUND ( 'NONE', #19202, .T. ) ;
#713 = DIRECTION ( 'NONE',  ( -1.402518428993831676E-16, 1.000000000000000000, -1.677918375355662166E-32 ) ) ;
#714 = CARTESIAN_POINT ( 'NONE',  ( 5.611423337425062385, 41.22389019960463230, 95.33621380123798872 ) ) ;
#715 = ORIENTED_EDGE ( 'NONE', *, *, #7235, .T. ) ;
#716 = CARTESIAN_POINT ( 'NONE',  ( 6.924055141134583202, 50.37376929599953712, 78.48669174070734300 ) ) ;
#717 = ORIENTED_EDGE ( 'NONE', *, *, #15127, .T. ) ;
#718 = DIRECTION ( 'NONE',  ( 1.334402673828313339E-16, 1.871524341742854397E-32, -1.000000000000000000 ) ) ;
#719 =( BOUNDED_SURFACE ( )  B_SPLINE_SURFACE ( 1, 2, ( 
 ( #14747, #19313, #8261, #13054, #13154, #16246, #9759, #1781, #14537, #7947, #6756, #17831, #19424, #6436, #8049, #4843, #13263, #9663, #21001, #1878, #18151, #14430, #19735, #9867, #4944, #11569, #8151, #14641, #5154, #3357, #8366, #11362, #19629, #14848, #16458, #12833, #1667, #18044, #68, #3466, #16144, #20900, #4729, #11675, #269, #11466, #3161, #1564, #3260, #19528, #6548, #17936, #9977, #1978, #5473, #12085, #2287, #8471, #10504, #6859, #19836, #5679, #479, #18248, #580, #3979, #8582, #6957, #11989, #18461, #14244, #11080, #9582, #13565, #583, #376, #5476, #8586, #18464 ),
 ( #18569, #5259, #18251, #5682, #15068, #7064, #10295, #482, #3982, #17089, #2402, #8903, #16872, #3671, #15392, #2086, #698, #5584, #6960, #10402, #3879, #12089, #13465, #14956, #11775, #11878, #6864, #7291, #13368, #5364, #20154, #2290, #10184, #20045, #13680, #8789, #13779, #15279, #12192, #18671, #4090, #9325, #7506, #17595, #20776, #10824, #12409, #20479, #1013, #18888, #6212, #2610, #13994, #15909, #11125, #9007, #12712, #2821, #18988, #4508, #1126, #7613, #19190, #17394, #1328, #4297, #14192, #7816, #9421, #5800, #2714, #6106, #9220, #11026, #9109, #15494, #905, #4604, #14301 ) ),
 .UNSPECIFIED., .F., .F., .T. ) 
 B_SPLINE_SURFACE_WITH_KNOTS ( ( 2, 2 ),
 ( 3, 2, 2, 2, 2, 2, 2, 2, 2, 2, 2, 2, 2, 2, 2, 2, 2, 2, 2, 2, 2, 2, 2, 2, 2, 2, 2, 2, 2, 2, 2, 2, 2, 2, 2, 2, 2, 2, 2, 3 ),
 ( 0.000000000000000000, 1.000000000000000000 ),
 ( 0.000000000000000000, 0.02500000000000000139, 0.05000000000000000278, 0.07499999999999999722, 0.1000000000000000056, 0.1250000000000000000, 0.1499999999999999944, 0.1749999999999999889, 0.2000000000000000111, 0.2250000000000000056, 0.2500000000000000000, 0.2750000000000000222, 0.2999999999999999889, 0.3250000000000000111, 0.3499999999999999778, 0.3750000000000000000, 0.4000000000000000222, 0.4249999999999999889, 0.4500000000000000111, 0.4749999999999999778, 0.5000000000000000000, 0.5250000000000000222, 0.5500000000000000444, 0.5749999999999999556, 0.5999999999999999778, 0.6250000000000000000, 0.6500000000000000222, 0.6750000000000000444, 0.6999999999999999556, 0.7249999999999999778, 0.7500000000000000000, 0.7750000000000000222, 0.8000000000000000444, 0.8249999999999999556, 0.8499999999999999778, 0.8750000000000000000, 0.9000000000000000222, 0.9250000000000000444, 0.9499999999999999556, 0.9600310108036838042 ),
 .UNSPECIFIED. ) 
 GEOMETRIC_REPRESENTATION_ITEM ( )  RATIONAL_B_SPLINE_SURFACE ( (
 ( 1.000000000000000000, 0.9238795325112867385, 1.000000000000000000, 0.9238795325112867385, 1.000000000000000000, 0.9238795325112867385, 1.000000000000000000, 0.9238795325112867385, 1.000000000000000000, 0.9238795325112867385, 1.000000000000000000, 0.9238795325112867385, 1.000000000000000000, 0.9238795325112867385, 1.000000000000000000, 0.9238795325112867385, 1.000000000000000000, 0.9238795325112867385, 1.000000000000000000, 0.9238795325112867385, 1.000000000000000000, 0.9238795325112867385, 1.000000000000000000, 0.9238795325112867385, 1.000000000000000000, 0.9238795325112867385, 1.000000000000000000, 0.9238795325112867385, 1.000000000000000000, 0.9238795325112867385, 1.000000000000000000, 0.9238795325112867385, 1.000000000000000000, 0.9238795325112867385, 1.000000000000000000, 0.9238795325112867385, 1.000000000000000000, 0.9238795325112867385, 1.000000000000000000, 0.9238795325112867385, 1.000000000000000000, 0.9238795325112867385, 1.000000000000000000, 0.9238795325112867385, 1.000000000000000000, 0.9238795325112867385, 1.000000000000000000, 0.9238795325112867385, 1.000000000000000000, 0.9238795325112867385, 1.000000000000000000, 0.9238795325112867385, 1.000000000000000000, 0.9238795325112867385, 1.000000000000000000, 0.9238795325112867385, 1.000000000000000000, 0.9238795325112867385, 1.000000000000000000, 0.9238795325112867385, 1.000000000000000000, 0.9238795325112867385, 1.000000000000000000, 0.9238795325112867385, 1.000000000000000000, 0.9238795325112867385, 1.000000000000000000, 0.9238795325112867385, 1.000000000000000000, 0.9238795325112867385, 1.000000000000000000, 0.9238795325112867385, 1.000000000000000000, 0.9238795325112867385, 1.000000000000000000, 0.9238795325112867385, 1.000000000000000000, 0.9694573907295700455, 0.9634246409442903669),
 ( 1.000000000000000000, 0.9238795325112867385, 1.000000000000000000, 0.9238795325112867385, 1.000000000000000000, 0.9238795325112867385, 1.000000000000000000, 0.9238795325112867385, 1.000000000000000000, 0.9238795325112867385, 1.000000000000000000, 0.9238795325112867385, 1.000000000000000000, 0.9238795325112867385, 1.000000000000000000, 0.9238795325112867385, 1.000000000000000000, 0.9238795325112867385, 1.000000000000000000, 0.9238795325112867385, 1.000000000000000000, 0.9238795325112867385, 1.000000000000000000, 0.9238795325112867385, 1.000000000000000000, 0.9238795325112867385, 1.000000000000000000, 0.9238795325112867385, 1.000000000000000000, 0.9238795325112867385, 1.000000000000000000, 0.9238795325112867385, 1.000000000000000000, 0.9238795325112867385, 1.000000000000000000, 0.9238795325112867385, 1.000000000000000000, 0.9238795325112867385, 1.000000000000000000, 0.9238795325112867385, 1.000000000000000000, 0.9238795325112867385, 1.000000000000000000, 0.9238795325112867385, 1.000000000000000000, 0.9238795325112867385, 1.000000000000000000, 0.9238795325112867385, 1.000000000000000000, 0.9238795325112867385, 1.000000000000000000, 0.9238795325112867385, 1.000000000000000000, 0.9238795325112867385, 1.000000000000000000, 0.9238795325112867385, 1.000000000000000000, 0.9238795325112867385, 1.000000000000000000, 0.9238795325112867385, 1.000000000000000000, 0.9238795325112867385, 1.000000000000000000, 0.9238795325112867385, 1.000000000000000000, 0.9238795325112867385, 1.000000000000000000, 0.9238795325112867385, 1.000000000000000000, 0.9238795325112867385, 1.000000000000000000, 0.9238795325112867385, 1.000000000000000000, 0.9238795325112867385, 1.000000000000000000, 0.9238795325112867385, 1.000000000000000000, 0.9694573907295700455, 0.9634246409442903669) ) ) 
 REPRESENTATION_ITEM ( '' )  SURFACE ( )  );
#720 = LINE ( 'NONE', #20278, #15623 ) ;
#721 = FACE_OUTER_BOUND ( 'NONE', #1347, .T. ) ;
#722 = LINE ( 'NONE', #4010, #13169 ) ;
#723 = DIRECTION ( 'NONE',  ( 1.540237394707284220E-16, 1.793354297423764243E-16, -1.000000000000000000 ) ) ;
#724 = CARTESIAN_POINT ( 'NONE',  ( 5.611423337425062385, 41.22389019960463230, 95.33621380123798872 ) ) ;
#725 = CARTESIAN_POINT ( 'NONE',  ( 8.792356959002002981, 41.14497608504091630, 76.18655208513948196 ) ) ;
#726 = CYLINDRICAL_SURFACE ( 'NONE', #8156, 1.399999999999998579 ) ;
#727 = CARTESIAN_POINT ( 'NONE',  ( 4.439499113014429454, 51.28417780296363304, 75.58280986828056314 ) ) ;
#728 = CARTESIAN_POINT ( 'NONE',  ( -2.077846259693550746, 39.65884927180063357, 91.97683880294496817 ) ) ;
#729 = AXIS2_PLACEMENT_3D ( 'NONE', #13957, #7460, #4047 ) ;
#730 = CARTESIAN_POINT ( 'NONE',  ( 1.658154530501163570, 36.04125148601230677, 76.86610350541322134 ) ) ;
#731 = ORIENTED_EDGE ( 'NONE', *, *, #14178, .T. ) ;
#732 = FACE_OUTER_BOUND ( 'NONE', #13452, .T. ) ;
#733 = AXIS2_PLACEMENT_3D ( 'NONE', #10034, #6712, #11945 ) ;
#734 = LINE ( 'NONE', #16201, #9841 ) ;
#735 = CARTESIAN_POINT ( 'NONE',  ( 2.522153740306494196, 49.81903562097208749, 67.21119304902339309 ) ) ;
#736 = CARTESIAN_POINT ( 'NONE',  ( -4.007802336140563249, 51.74101282905964894, 79.45569801420249689 ) ) ;
#737 = CARTESIAN_POINT ( 'NONE',  ( 3.460444912181559474, 49.25145096859824889, 94.39871380123798872 ) ) ;
#738 = CARTESIAN_POINT ( 'NONE',  ( -4.850396850989173281, 37.19025346873809923, 77.31947969467269388 ) ) ;
#739 = CARTESIAN_POINT ( 'NONE',  ( 28.52215374030650352, 44.16218137147969003, 105.5543387995309956 ) ) ;
#740 = CARTESIAN_POINT ( 'NONE',  ( 0.5838706545074757726, 52.36194911346490954, 78.93669174070734584 ) ) ;
#741 = EDGE_CURVE ( 'NONE', #19585, #19846, #11459, .T. ) ;
#742 = CARTESIAN_POINT ( 'NONE',  ( 5.722153740306477054, 44.16218185475116798, 93.64411094854725093 ) ) ;
#743 = EDGE_LOOP ( 'NONE', ( #1066, #16870, #8896, #16455 ) ) ;
#744 = ORIENTED_EDGE ( 'NONE', *, *, #6572, .T. ) ;
#745 = AXIS2_PLACEMENT_3D ( 'NONE', #16885, #20171, #18584 ) ;
#746 = CARTESIAN_POINT ( 'NONE',  ( 8.553273006160548420, 42.79284436168489947, 79.20437336408532758 ) ) ;
#747 = FACE_OUTER_BOUND ( 'NONE', #12608, .T. ) ;
#748 = CARTESIAN_POINT ( 'NONE',  ( 8.930560609631596591, 41.55918119345393080, 76.05553801048951357 ) ) ;
#749 = VECTOR ( 'NONE', #20984, 1000.000000000000000 ) ;
#750 = CARTESIAN_POINT ( 'NONE',  ( -5.784195910403845176, 44.99242805365518194, 94.78933880123798872 ) ) ;
#751 = LINE ( 'NONE', #13732, #1966 ) ;
#752 = DIRECTION ( 'NONE',  ( -0.000000000000000000, -3.469446951953617147E-16, -1.000000000000000000 ) ) ;
#753 = CARTESIAN_POINT ( 'NONE',  ( 5.025485839985549319, 41.56218137147963887, 92.28933880294496817 ) ) ;
#754 = FACE_OUTER_BOUND ( 'NONE', #10086, .T. ) ;
#755 = EDGE_CURVE ( 'NONE', #2672, #14271, #8781, .T. ) ;
#756 = CARTESIAN_POINT ( 'NONE',  ( -7.720740609617425143, 47.25708002984855227, 78.10358362899698648 ) ) ;
#757 = CARTESIAN_POINT ( 'NONE',  ( 3.460444912181559474, 49.25145096859824889, 94.24246380123798872 ) ) ;
#758 = CIRCLE ( 'NONE', #14682, 4.000000000000000000 ) ;
#759 = CARTESIAN_POINT ( 'NONE',  ( 6.851319717782478946, 37.86899943589613571, 76.12774863075016185 ) ) ;
#760 = CARTESIAN_POINT ( 'NONE',  ( 5.791714832554497150, 51.21018346849771063, 78.93490712750880789 ) ) ;
#761 = VECTOR ( 'NONE', #8337, 1000.000000000000000 ) ;
#762 = CARTESIAN_POINT ( 'NONE',  ( 2.522153740306507963, 49.16218137147969003, 66.55433879953099563 ) ) ;
#763 = EDGE_CURVE ( 'NONE', #2000, #9068, #9535, .T. ) ;
#764 = ORIENTED_EDGE ( 'NONE', *, *, #13645, .F. ) ;
#765 = DIRECTION ( 'NONE',  ( 0.000000000000000000, 0.000000000000000000, -1.000000000000000000 ) ) ;
#766 = CARTESIAN_POINT ( 'NONE',  ( -2.416137431568557314, 39.07291177436112406, 91.11746380123798872 ) ) ;
#767 = EDGE_LOOP ( 'NONE', ( #8584, #12522, #398, #10507 ) ) ;
#768 = EDGE_CURVE ( 'NONE', #4756, #9174, #10932, .T. ) ;
#769 = FACE_OUTER_BOUND ( 'NONE', #9422, .T. ) ;
#770 = ADVANCED_FACE ( 'NONE', ( #9332 ), #13036, .T. ) ;
#771 = CARTESIAN_POINT ( 'NONE',  ( 1.215246153217547365, 50.28109722957945849, 59.67325465763076409 ) ) ;
#772 = CARTESIAN_POINT ( 'NONE',  ( -4.274069566951154364, 51.55074801458793132, 79.52610421797659512 ) ) ;
#773 = CARTESIAN_POINT ( 'NONE',  ( 10.77494014480653561, 42.76218137147968434, 66.20574467885103331 ) ) ;
#774 = CARTESIAN_POINT ( 'NONE',  ( -8.192078482032012943, 42.93655631659661509, 75.45433879953087342 ) ) ;
#775 = CARTESIAN_POINT ( 'NONE',  ( 0.5221537403065364957, 44.16218137147969003, 123.5543387995310098 ) ) ;
#776 = ORIENTED_EDGE ( 'NONE', *, *, #7548, .F. ) ;
#777 = CARTESIAN_POINT ( 'NONE',  ( 5.327855396560547518, 50.80644620442382831, 77.95494770374325810 ) ) ;
#778 = VECTOR ( 'NONE', #3824, 1000.000000000000000 ) ;
#779 = ORIENTED_EDGE ( 'NONE', *, *, #2877, .T. ) ;
#780 = DIRECTION ( 'NONE',  ( -0.5735764363510442720, 0.8191520442889930198, -9.299032798180124612E-17 ) ) ;
#781 = CARTESIAN_POINT ( 'NONE',  ( 4.973101328672442811, 51.81486028805201727, 77.67439681936272677 ) ) ;
#782 = FACE_OUTER_BOUND ( 'NONE', #1025, .T. ) ;
#783 = EDGE_CURVE ( 'NONE', #5897, #5621, #16225, .T. ) ;
#784 = DIRECTION ( 'NONE',  ( 1.540237394707284220E-16, 1.793354297423764243E-16, -1.000000000000000000 ) ) ;
#785 = CARTESIAN_POINT ( 'NONE',  ( 5.807634474669838731, 51.19842427014940967, 79.54761434581399726 ) ) ;
#786 = DIRECTION ( 'NONE',  ( 0.7071067811865539010, -3.662367542345418158E-17, -0.7071067811865411334 ) ) ;
#787 = CARTESIAN_POINT ( 'NONE',  ( 3.394633603133437205, 39.16678578622979501, 95.40913158822179696 ) ) ;
#788 = CARTESIAN_POINT ( 'NONE',  ( 11.22215374030650281, 42.96218137147968008, 57.80715055817105252 ) ) ;
#789 = ORIENTED_EDGE ( 'NONE', *, *, #20431, .T. ) ;
#790 = CARTESIAN_POINT ( 'NONE',  ( 8.804944317620234884, 41.18270119734690837, 78.86399424569901839 ) ) ;
#791 = VERTEX_POINT ( 'NONE', #19512 ) ;
#792 = AXIS2_PLACEMENT_3D ( 'NONE', #14982, #5280, #2111 ) ;
#793 = DIRECTION ( 'NONE',  ( -0.000000000000000000, -0.000000000000000000, 1.000000000000000000 ) ) ;
#794 = CARTESIAN_POINT ( 'NONE',  ( 6.102441102155617969, 43.42752260303680600, 93.30496379953098085 ) ) ;
#795 = CARTESIAN_POINT ( 'NONE',  ( -8.068594480573938910, 42.12297466537643942, 77.08187429197492690 ) ) ;
#796 = ORIENTED_EDGE ( 'NONE', *, *, #371, .F. ) ;
#797 = CARTESIAN_POINT ( 'NONE',  ( 6.198496396448986090, 45.68315280215533392, 94.24246380123798872 ) ) ;
#798 = CARTESIAN_POINT ( 'NONE',  ( 29.03948732994507864, 43.16218137147969003, 74.70433879953100131 ) ) ;
#799 = VERTEX_POINT ( 'NONE', #152 ) ;
#800 = CARTESIAN_POINT ( 'NONE',  ( 0.5221537403065010796, 44.16218137147968292, 78.32492703482499508 ) ) ;
#801 = CARTESIAN_POINT ( 'NONE',  ( -1.677846259693499542, 47.73989013547934945, 45.55433879953098852 ) ) ;
#802 = ADVANCED_FACE ( 'NONE', ( #9845 ), #1442, .T. ) ;
#803 = ORIENTED_EDGE ( 'NONE', *, *, #2329, .T. ) ;
#804 = FACE_BOUND ( 'NONE', #6425, .T. ) ;
#805 = B_SPLINE_CURVE_WITH_KNOTS ( 'NONE', 3,
 ( #15016, #8846, #2143, #7341, #12045, #10458, #13833, #20311, #7014, #436, #6917, #7122, #13421, #16825, #19891, #2243, #4147, #10243, #13514, #13624, #16720, #11937, #18733, #5742, #5311, #19991 ),
 .UNSPECIFIED., .F., .F.,
 ( 4, 2, 2, 2, 2, 2, 2, 2, 2, 2, 2, 2, 4 ),
 ( 0.000000000000000000, 0.001364898262398260478, 0.002047347393597397439, 0.002729796524796534399, 0.004094694787194807888, 0.004777143918393935741, 0.005459593049593063595, 0.006824491311991337517, 0.007506940443190486187, 0.008189389574389634857, 0.008871838705588783527, 0.009554287836787932198, 0.01091918609918624342 ),
 .UNSPECIFIED. ) ;
#806 = ORIENTED_EDGE ( 'NONE', *, *, #4198, .F. ) ;
#807 = DIRECTION ( 'NONE',  ( 2.043266227890062685E-16, 0.7071067811865451302, -0.7071067811865500152 ) ) ;
#808 = DIRECTION ( 'NONE',  ( 0.000000000000000000, 0.000000000000000000, 1.000000000000000000 ) ) ;
#809 = ADVANCED_FACE ( 'NONE', ( #8244 ), #7929, .T. ) ;
#810 = EDGE_CURVE ( 'NONE', #4828, #14664, #20355, .T. ) ;
#811 = EDGE_CURVE ( 'NONE', #2938, #15510, #6634, .T. ) ;
#812 = AXIS2_PLACEMENT_3D ( 'NONE', #507, #5716, #3806 ) ;
#813 = CONTEXT_DEPENDENT_SHAPE_REPRESENTATION ( #3415, #5466 ) ;
#814 = CARTESIAN_POINT ( 'NONE',  ( -4.523256899386018937, 37.70324430649279179, 76.12782976279942204 ) ) ;
#815 = CARTESIAN_POINT ( 'NONE',  ( 2.232254456934871456, 39.46371826755015633, 93.73558879953097289 ) ) ;
#816 = CARTESIAN_POINT ( 'NONE',  ( -7.280826702657820171, 41.64048047902432614, 78.01850061686013760 ) ) ;
#817 = CARTESIAN_POINT ( 'NONE',  ( 1.767938056577025741, 52.20425435525031332, 75.65494847458032268 ) ) ;
#818 = EDGE_LOOP ( 'NONE', ( #19736, #7395, #18989, #273 ) ) ;
#819 = CARTESIAN_POINT ( 'NONE',  ( 6.398363615859712361, 50.76207644957375464, 75.46588380158773646 ) ) ;
#820 = CARTESIAN_POINT ( 'NONE',  ( 2.108290839596759003, 51.34989793853182505, 77.84551527011910821 ) ) ;
#821 = CARTESIAN_POINT ( 'NONE',  ( -0.9988176903691428077, 49.83852402762217082, 92.05496380123798872 ) ) ;
#822 = ORIENTED_EDGE ( 'NONE', *, *, #8018, .F. ) ;
#823 = CARTESIAN_POINT ( 'NONE',  ( 6.923174433796239313, 50.37441983903331533, 78.52964612251847143 ) ) ;
#824 = ORIENTED_EDGE ( 'NONE', *, *, #3471, .T. ) ;
#825 = DIRECTION ( 'NONE',  ( -0.9429220365244121993, 0.3330135628418984250, -8.551124769255302663E-17 ) ) ;
#826 = CARTESIAN_POINT ( 'NONE',  ( 0.5221537403065008576, 44.16218137147968292, 80.45433879953087342 ) ) ;
#827 = CARTESIAN_POINT ( 'NONE',  ( -1.187946976321871073, 48.86064447540922373, 91.86058879953097289 ) ) ;
#828 = CARTESIAN_POINT ( 'NONE',  ( 6.828503391016846891, 43.33193468930419101, 92.75808880123807398 ) ) ;
#829 = CARTESIAN_POINT ( 'NONE',  ( -7.359991238862622076, 41.90117226254449179, 78.84683685324785074 ) ) ;
#830 = CARTESIAN_POINT ( 'NONE',  ( -7.531346616919285530, 42.61233131736031510, 79.37808970707625633 ) ) ;
#831 = EDGE_CURVE ( 'NONE', #13896, #1135, #9541, .T. ) ;
#832 = CARTESIAN_POINT ( 'NONE',  ( -6.210882734309923769, 46.73118581782181025, 75.45433879953087342 ) ) ;
#833 = CARTESIAN_POINT ( 'NONE',  ( 8.817118105929894867, 41.21918681320168787, 76.01674029036281866 ) ) ;
#834 = FACE_OUTER_BOUND ( 'NONE', #13780, .T. ) ;
#835 = DIRECTION ( 'NONE',  ( 0.5954989751681698529, -0.8033560671169786005, -5.234922652618075161E-17 ) ) ;
#836 = CARTESIAN_POINT ( 'NONE',  ( 1.868012774839550749, 39.13936707477651566, 92.13308880294498238 ) ) ;
#837 = CARTESIAN_POINT ( 'NONE',  ( -7.945066593710369496, 41.73949022789241781, 78.79490040793942285 ) ) ;
#838 = ORIENTED_EDGE ( 'NONE', *, *, #17686, .F. ) ;
#839 = CARTESIAN_POINT ( 'NONE',  ( 8.950958007118590132, 41.62031348770922534, 78.64183653779139149 ) ) ;
#840 = ORIENTED_EDGE ( 'NONE', *, *, #1689, .T. ) ;
#841 = DIRECTION ( 'NONE',  ( 1.000000000000000000, 0.000000000000000000, -0.000000000000000000 ) ) ;
#842 = CARTESIAN_POINT ( 'NONE',  ( -0.1709386726045625804, 50.28109722957944427, 67.67325465763074988 ) ) ;
#843 = DIRECTION ( 'NONE',  ( -9.598494438985367424E-18, 5.922860397471809309E-17, -1.000000000000000000 ) ) ;
#844 = CARTESIAN_POINT ( 'NONE',  ( -3.350035803220276609, 49.20851703305431357, 92.13308880123798872 ) ) ;
#845 = CARTESIAN_POINT ( 'NONE',  ( -4.718161399584266391, 37.09257646755418847, 75.97198585835440099 ) ) ;
#846 = FACE_OUTER_BOUND ( 'NONE', #4937, .T. ) ;
#847 = LINE ( 'NONE', #20417, #14344 ) ;
#848 = EDGE_CURVE ( 'NONE', #7921, #15771, #17815, .T. ) ;
#849 = CARTESIAN_POINT ( 'NONE',  ( 5.524900579399185219, 50.65415293276860353, 78.06587361566768379 ) ) ;
#850 = ORIENTED_EDGE ( 'NONE', *, *, #17509, .F. ) ;
#851 = ORIENTED_EDGE ( 'NONE', *, *, #831, .F. ) ;
#852 = PRODUCT_DEFINITION_CONTEXT ( 'detailed design', #2327, 'design' ) ;
#853 = CARTESIAN_POINT ( 'NONE',  ( 8.162892682119435861, 41.62284976526770208, 79.54845644658969661 ) ) ;
#854 = CARTESIAN_POINT ( 'NONE',  ( -4.074436747594614161, 36.61708299794013044, 75.46341390175899733 ) ) ;
#855 = DIRECTION ( 'NONE',  ( -1.000000000000000000, -1.402518428993831676E-16, -1.196361017915039239E-16 ) ) ;
#856 = CARTESIAN_POINT ( 'NONE',  ( 0.5838706545074757726, 52.36194911346490954, 78.93669174070734584 ) ) ;
#857 = CARTESIAN_POINT ( 'NONE',  ( 5.561379608955574483, 51.38032281970146897, 76.90580938776616904 ) ) ;
#858 = CARTESIAN_POINT ( 'NONE',  ( 9.155505153612395475, 42.23335426198017473, 78.07975471416389723 ) ) ;
#859 = CARTESIAN_POINT ( 'NONE',  ( -3.943187491250720544, 40.73580453397070755, 91.89871380294498238 ) ) ;
#860 = LINE ( 'NONE', #18737, #17293 ) ;
#861 = CARTESIAN_POINT ( 'NONE',  ( -7.670684956156135215, 47.40709999874347602, 78.27541057140679470 ) ) ;
#862 = DIRECTION ( 'NONE',  ( 1.540237394707284220E-16, 1.793354297423764243E-16, -1.000000000000000000 ) ) ;
#863 = EDGE_CURVE ( 'NONE', #9302, #16784, #3241, .T. ) ;
#864 = CARTESIAN_POINT ( 'NONE',  ( 0.5221537403065118488, 48.16218137147969003, 45.55433879953100273 ) ) ;
#865 = ORIENTED_EDGE ( 'NONE', *, *, #3090, .T. ) ;
#866 = CARTESIAN_POINT ( 'NONE',  ( 5.410205795499257064, 50.73735288404611055, 77.28904345712264501 ) ) ;
#867 = VERTEX_POINT ( 'NONE', #3450 ) ;
#868 = CARTESIAN_POINT ( 'NONE',  ( -4.796459876899764829, 51.17746702502860501, 78.71090438869831019 ) ) ;
#869 = CARTESIAN_POINT ( 'NONE',  ( 1.256812508749381774, 49.74246873332880625, 95.17996380294498238 ) ) ;
#870 = ORIENTED_EDGE ( 'NONE', *, *, #20402, .T. ) ;
#871 = DIRECTION ( 'NONE',  ( -1.000000000000000000, 0.000000000000000000, -1.621236893436268647E-16 ) ) ;
#872 = DIRECTION ( 'NONE',  ( -0.5941461771851691553, -0.8043570849667760481, -2.357623395011396791E-16 ) ) ;
#873 = EDGE_CURVE ( 'NONE', #57, #5204, #20786, .T. ) ;
#874 = CARTESIAN_POINT ( 'NONE',  ( -3.572718533232662530, 51.13213220290453620, 79.45569801420249689 ) ) ;
#875 = CARTESIAN_POINT ( 'NONE',  ( -6.792737292293177909, 47.86790251333490431, 72.45433879953087342 ) ) ;
#876 = CARTESIAN_POINT ( 'NONE',  ( 5.201148050424325042, 50.89177541897332446, 76.94115191089467487 ) ) ;
#877 = FACE_OUTER_BOUND ( 'NONE', #6596, .T. ) ;
#878 = ORIENTED_EDGE ( 'NONE', *, *, #3983, .T. ) ;
#879 = LINE ( 'NONE', #2373, #10565 ) ;
#880 = VERTEX_POINT ( 'NONE', #9961 ) ;
#881 = CARTESIAN_POINT ( 'NONE',  ( -3.477846259693496478, 44.16218137147969003, 105.5543387995310098 ) ) ;
#882 = CARTESIAN_POINT ( 'NONE',  ( 4.539372959821318609, 52.13523796247791608, 76.58963291717793709 ) ) ;
#883 = CARTESIAN_POINT ( 'NONE',  ( 6.828109521384686076, 50.44464046038347504, 77.45110917081549928 ) ) ;
#884 = CARTESIAN_POINT ( 'NONE',  ( 5.611423337425062385, 41.22389019960463230, 92.83621380123797451 ) ) ;
#885 = CARTESIAN_POINT ( 'NONE',  ( -7.833107574997801414, 41.39546341374030902, 76.33867328066237690 ) ) ;
#886 = CARTESIAN_POINT ( 'NONE',  ( 8.868817592801745420, 41.37413345511091478, 75.97198585835440099 ) ) ;
#887 = CARTESIAN_POINT ( 'NONE',  ( -4.174946515328806562, 37.44075729451967760, 78.12452307498179493 ) ) ;
#888 = CARTESIAN_POINT ( 'NONE',  ( 6.489847418355314979, 49.78593742637539776, 78.48669174070734300 ) ) ;
#889 = VERTEX_POINT ( 'NONE', #9743 ) ;
#890 = CARTESIAN_POINT ( 'NONE',  ( 8.787829143201873805, 41.13140593384864729, 78.45948585835439815 ) ) ;
#891 = ORIENTED_EDGE ( 'NONE', *, *, #5714, .F. ) ;
#892 = CARTESIAN_POINT ( 'NONE',  ( 27.03948732994508930, 36.35905713404685713, 76.90433879953101837 ) ) ;
#893 = CARTESIAN_POINT ( 'NONE',  ( -4.500660556396669065, 42.81632233694663370, 92.75808879953098085 ) ) ;
#894 = CARTESIAN_POINT ( 'NONE',  ( -7.364103761167730688, 42.34575162834247664, 77.08187429197492690 ) ) ;
#895 = VERTEX_POINT ( 'NONE', #1649 ) ;
#896 = CARTESIAN_POINT ( 'NONE',  ( 1.352400422481993658, 50.46853102219002096, 93.22683880123798872 ) ) ;
#897 = LINE ( 'NONE', #15589, #7222 ) ;
#898 = CARTESIAN_POINT ( 'NONE',  ( 0.3326973149608335456, 52.96014171822455552, 77.76169174070734869 ) ) ;
#899 = VERTEX_POINT ( 'NONE', #11241 ) ;
#900 = DIRECTION ( 'NONE',  ( -0.3165065846431170393, -0.9485903129789747812, 0.000000000000000000 ) ) ;
#901 = EDGE_CURVE ( 'NONE', #14294, #3149, #17917, .T. ) ;
#902 = FACE_OUTER_BOUND ( 'NONE', #1834, .T. ) ;
#903 = ORIENTED_EDGE ( 'NONE', *, *, #17975, .F. ) ;
#904 = CARTESIAN_POINT ( 'NONE',  ( 11.22215374030650281, 42.76218137147968434, 78.80433879953099563 ) ) ;
#905 = CARTESIAN_POINT ( 'NONE',  ( 5.611423337425062385, 41.22389019960463230, 90.33621380123798872 ) ) ;
#906 = ORIENTED_EDGE ( 'NONE', *, *, #9778, .F. ) ;
#907 = CARTESIAN_POINT ( 'NONE',  ( -4.450561708517716930, 41.89428209290792182, 92.45433879953095868 ) ) ;
#908 = CARTESIAN_POINT ( 'NONE',  ( 29.63948732994508006, 43.16218137147969003, 74.70433879953100131 ) ) ;
#909 = AXIS2_PLACEMENT_3D ( 'NONE', #9327, #1226, #1330 ) ;
#910 = CONTEXT_DEPENDENT_SHAPE_REPRESENTATION ( #8452, #10432 ) ;
#911 = CARTESIAN_POINT ( 'NONE',  ( -3.568560454108619773, 36.24341255788211669, 78.11242031084098869 ) ) ;
#913 = EDGE_CURVE ( 'NONE', #16685, #14370, #19197, .T. ) ;
#912 = CARTESIAN_POINT ( 'NONE',  ( 5.428282431822193388, 36.85214909206928269, 76.61095391776262886 ) ) ;
#914 = CYLINDRICAL_SURFACE ( 'NONE', #4488, 6.000000000000002665 ) ;
#915 = EDGE_CURVE ( 'NONE', #7365, #682, #8745, .T. ) ;
#916 = ORIENTED_EDGE ( 'NONE', *, *, #8534, .T. ) ;
#917 = CARTESIAN_POINT ( 'NONE',  ( 1.478628313566038077, 52.95937378012966690, 75.49332451037695080 ) ) ;
#918 = ORIENTED_EDGE ( 'NONE', *, *, #10957, .F. ) ;
#919 = FACE_BOUND ( 'NONE', #656, .T. ) ;
#920 = EDGE_CURVE ( 'NONE', #6129, #19774, #17602, .T. ) ;
#921 = CARTESIAN_POINT ( 'NONE',  ( 1.652727357819364418, 35.35299279957455099, 76.16022115247204738 ) ) ;
#922 = CARTESIAN_POINT ( 'NONE',  ( 5.568489401881125289, 48.03437091500646261, 93.07058880123797451 ) ) ;
#923 = ADVANCED_FACE ( 'NONE', ( #3145 ), #3031, .F. ) ;
#924 = ORIENTED_EDGE ( 'NONE', *, *, #9750, .F. ) ;
#925 = CIRCLE ( 'NONE', #3632, 8.199999999999995737 ) ;
#926 = CARTESIAN_POINT ( 'NONE',  ( -4.383323755399650246, 50.73378672401133826, 75.36197610833401939 ) ) ;
#927 = ORIENTED_EDGE ( 'NONE', *, *, #5864, .F. ) ;
#928 = FACE_OUTER_BOUND ( 'NONE', #9385, .T. ) ;
#929 = DIRECTION ( 'NONE',  ( 1.540237394707284220E-16, 1.793354297423764243E-16, -1.000000000000000000 ) ) ;
#930 = CARTESIAN_POINT ( 'NONE',  ( 2.232254456934872788, 39.46371826755015633, 91.23558879953097289 ) ) ;
#931 = CARTESIAN_POINT ( 'NONE',  ( -5.412716252285424190, 48.91899944357702879, 72.45433879953087342 ) ) ;
#932 = CARTESIAN_POINT ( 'NONE',  ( -7.018774656858025374, 41.28963458989208846, 79.50989352969267543 ) ) ;
#933 = CARTESIAN_POINT ( 'NONE',  ( 30.43948732994507722, 36.35905713404685002, 74.70433879953098710 ) ) ;
#934 = CARTESIAN_POINT ( 'NONE',  ( 1.514255888186008425, 52.36218137147968577, 52.53721119516358584 ) ) ;
#935 = FACE_OUTER_BOUND ( 'NONE', #5234, .T. ) ;
#936 = AXIS2_PLACEMENT_3D ( 'NONE', #5717, #18816, #20979 ) ;
#937 = CARTESIAN_POINT ( 'NONE',  ( -5.271099104061234719, 49.91853162867187166, 75.88700421999355683 ) ) ;
#938 = CARTESIAN_POINT ( 'NONE',  ( 5.080928206799192992, 51.73521291671138300, 75.47011219584838670 ) ) ;
#939 = CARTESIAN_POINT ( 'NONE',  ( 4.987494971863720927, 47.58855820898865829, 93.77371380294498238 ) ) ;
#940 = AXIS2_PLACEMENT_3D ( 'NONE', #20181, #13804, #18494 ) ;
#941 = CARTESIAN_POINT ( 'NONE',  ( -7.590962929491896105, 40.75019128785367428, 79.42781143817570921 ) ) ;
#942 = ORIENTED_EDGE ( 'NONE', *, *, #14551, .F. ) ;
#943 = CARTESIAN_POINT ( 'NONE',  ( 8.336228674048411946, 41.69800626661804444, 78.91042349786003740 ) ) ;
#944 = ORIENTED_EDGE ( 'NONE', *, *, #19238, .F. ) ;
#945 = CARTESIAN_POINT ( 'NONE',  ( -7.610866399937288307, 43.11623716858539979, 75.65823358996551917 ) ) ;
#946 = DIRECTION ( 'NONE',  ( -0.000000000000000000, -0.000000000000000000, 1.000000000000000000 ) ) ;
#947 = EDGE_CURVE ( 'NONE', #4394, #14370, #1546, .T. ) ;
#948 = CARTESIAN_POINT ( 'NONE',  ( -3.713457647669470063, 51.95134076679423174, 79.29276450469329518 ) ) ;
#949 = SURFACE_STYLE_USAGE ( .BOTH. , #20520 ) ;
#950 = AXIS2_PLACEMENT_3D ( 'NONE', #20455, #3858, #5889 ) ;
#951 = CARTESIAN_POINT ( 'NONE',  ( 0.5221537403065010796, 44.16218137147968292, 78.25433879953088478 ) ) ;
#952 = CARTESIAN_POINT ( 'NONE',  ( -8.289887965425112526, 42.82811778982430440, 78.89751519991851580 ) ) ;
#953 = CARTESIAN_POINT ( 'NONE',  ( 0.5221537403065011906, 44.16218137147968292, 77.43080938776617472 ) ) ;
#954 = CARTESIAN_POINT ( 'NONE',  ( -4.196599071979020046, 37.46195532796716776, 76.05537227506185616 ) ) ;
#955 = ORIENTED_EDGE ( 'NONE', *, *, #12761, .T. ) ;
#956 = ORIENTED_EDGE ( 'NONE', *, *, #20825, .F. ) ;
#957 = B_SPLINE_CURVE_WITH_KNOTS ( 'NONE', 3,
 ( #8213, #3213, #17789, #20957, #4896, #16196, #6391, #19271, #20859, #1410, #4684, #11207 ),
 .UNSPECIFIED., .F., .F.,
 ( 4, 2, 2, 2, 2, 4 ),
 ( 0.000000000000000000, 0.0001994714521133825950, 0.0003989429042267651901, 0.0007978858084534908067, 0.001196828712680216749, 0.001595771616906942365 ),
 .UNSPECIFIED. ) ;
#958 = CARTESIAN_POINT ( 'NONE',  ( 8.288346550782289768, 41.53027563821294166, 78.93576830848654424 ) ) ;
#959 = FACE_OUTER_BOUND ( 'NONE', #20377, .T. ) ;
#960 = FACE_OUTER_BOUND ( 'NONE', #10254, .T. ) ;
#961 = PLANE ( 'NONE',  #7240 ) ;
#962 = CARTESIAN_POINT ( 'NONE',  ( 5.599756831756513620, 51.35197511114724733, 78.21422674182478829 ) ) ;
#963 = CARTESIAN_POINT ( 'NONE',  ( 8.370724156415352724, 42.24573387831544835, 78.12791555553386047 ) ) ;
#964 = CARTESIAN_POINT ( 'NONE',  ( -5.058133621542618030, 44.89684013992257405, 92.99246380294498238 ) ) ;
#965 = CIRCLE ( 'NONE', #19972, 4.199999999999999289 ) ;
#966 = CARTESIAN_POINT ( 'NONE',  ( -4.572866156349838285, 51.33723891144499163, 75.97260225988416948 ) ) ;
#967 = CARTESIAN_POINT ( 'NONE',  ( -7.727022169037351063, 47.23825379777235156, 77.78596583901244799 ) ) ;
#968 = CARTESIAN_POINT ( 'NONE',  ( -4.524181921268124462, 40.28999182795290324, 91.03933880123798872 ) ) ;
#969 = CARTESIAN_POINT ( 'NONE',  ( 6.880792506138228681, 37.89005961138749967, 76.49840989696882332 ) ) ;
#970 = VERTEX_POINT ( 'NONE', #12049 ) ;
#971 = CARTESIAN_POINT ( 'NONE',  ( 5.929557977968517690, 51.10836428964097422, 77.10005730845655592 ) ) ;
#972 = VERTEX_POINT ( 'NONE', #15550 ) ;
#973 = DIRECTION ( 'NONE',  ( 0.000000000000000000, 0.000000000000000000, -1.000000000000000000 ) ) ;
#974 = CARTESIAN_POINT ( 'NONE',  ( -5.058133621542618030, 44.89684013992257405, 92.99246380294498238 ) ) ;
#975 = ORIENTED_EDGE ( 'NONE', *, *, #16774, .T. ) ;
#976 = CARTESIAN_POINT ( 'NONE',  ( -4.498303996637021740, 46.81144376258747997, 95.05433879953096721 ) ) ;
#977 = AXIS2_PLACEMENT_3D ( 'NONE', #6001, #1220, #20666 ) ;
#978 = CARTESIAN_POINT ( 'NONE',  ( -0.9388773962491537839, 52.84004908296358849, 72.45433879953087342 ) ) ;
#979 = LINE ( 'NONE', #5557, #2694 ) ;
#980 = DIRECTION ( 'NONE',  ( -1.000000000000000000, -1.402518428993831676E-16, -1.196361017915039239E-16 ) ) ;
#981 = CARTESIAN_POINT ( 'NONE',  ( 0.3849377270197763545, 52.36105381785655055, 77.46089079190313953 ) ) ;
#982 = CARTESIAN_POINT ( 'NONE',  ( -3.532917577324401925, 36.21708460058427193, 78.46683879953087626 ) ) ;
#983 = VERTEX_POINT ( 'NONE', #9062 ) ;
#984 = CARTESIAN_POINT ( 'NONE',  ( 4.048141534226263438, 36.75897868094575216, 79.45433879953087342 ) ) ;
#985 = EDGE_CURVE ( 'NONE', #165, #15850, #4155, .T. ) ;
#986 = CARTESIAN_POINT ( 'NONE',  ( 5.052198367669454626, 48.31320248322254685, 93.26683879782399345 ) ) ;
#987 = ORIENTED_EDGE ( 'NONE', *, *, #14448, .T. ) ;
#988 = CARTESIAN_POINT ( 'NONE',  ( -4.047219024143313248, 37.35069009299581211, 75.37207009874634878 ) ) ;
#989 = PLANE ( 'NONE',  #4341 ) ;
#990 = CARTESIAN_POINT ( 'NONE',  ( -7.149724537181753270, 47.05990690267743304, 79.05973021912267029 ) ) ;
#991 = FACE_OUTER_BOUND ( 'NONE', #3571, .T. ) ;
#992 = CARTESIAN_POINT ( 'NONE',  ( -4.432998774651716545, 37.62853090491852015, 77.91271439283131883 ) ) ;
#993 = CARTESIAN_POINT ( 'NONE',  ( 6.352851448254905442, 49.92817053755964452, 79.12994158702615266 ) ) ;
#994 = VECTOR ( 'NONE', #12378, 1000.000000000000000 ) ;
#995 = ORIENTED_EDGE ( 'NONE', *, *, #8965, .F. ) ;
#996 = CARTESIAN_POINT ( 'NONE',  ( 4.621588727139584130, 51.26391586304784198, 77.68963291717793140 ) ) ;
#997 = ORIENTED_EDGE ( 'NONE', *, *, #416, .T. ) ;
#998 = AXIS2_PLACEMENT_3D ( 'NONE', #18909, #10848, #17317 ) ;
#999 = CARTESIAN_POINT ( 'NONE',  ( -4.652687709939232086, 51.28020135170361016, 75.36022115247205022 ) ) ;
#1000 = CARTESIAN_POINT ( 'NONE',  ( -2.416137431568557314, 39.07291177436112406, 95.02371380123797451 ) ) ;
#1001 = CARTESIAN_POINT ( 'NONE',  ( -7.933076142375738549, 41.69442312082315993, 77.67112630499640602 ) ) ;
#1002 = EDGE_LOOP ( 'NONE', ( #17060, #19303, #20211, #3071 ) ) ;
#1003 = VECTOR ( 'NONE', #13053, 1000.000000000000000 ) ;
#1004 = CARTESIAN_POINT ( 'NONE',  ( 3.460444912181559474, 49.25145096859824889, 94.39871380123798872 ) ) ;
#1005 = CARTESIAN_POINT ( 'NONE',  ( -4.812088799398940075, 42.22067586467031930, 95.06371379782397923 ) ) ;
#1006 = CARTESIAN_POINT ( 'NONE',  ( 31.22215374030650281, 45.56218137147968861, 78.80433879953099563 ) ) ;
#1007 = CARTESIAN_POINT ( 'NONE',  ( 4.597212664172372953, 36.25829706351294135, 75.77524573853747825 ) ) ;
#1008 = DIRECTION ( 'NONE',  ( 1.000000000000000000, 0.000000000000000000, 0.000000000000000000 ) ) ;
#1009 = ADVANCED_FACE ( 'NONE', ( #7454 ), #4426, .F. ) ;
#1010 = EDGE_LOOP ( 'NONE', ( #9860, #18448, #3398, #16229 ) ) ;
#1011 = CARTESIAN_POINT ( 'NONE',  ( 29.77115333998618496, 40.36218137147969287, 87.85433879953102121 ) ) ;
#1012 = AXIS2_PLACEMENT_3D ( 'NONE', #7652, #20296, #841 ) ;
#1013 = CARTESIAN_POINT ( 'NONE',  ( -2.416137431568557314, 39.07291177436112406, 92.52371380123797451 ) ) ;
#1014 = EDGE_CURVE ( 'NONE', #1329, #11872, #20433, .T. ) ;
#1015 = VERTEX_POINT ( 'NONE', #4043 ) ;
#1016 = CARTESIAN_POINT ( 'NONE',  ( -5.111781840388389675, 44.40467396443471415, 92.45433879953098710 ) ) ;
#1017 = CARTESIAN_POINT ( 'NONE',  ( 5.094470189521428161, 37.35527774201511875, 76.21970569554892450 ) ) ;
#1018 = CARTESIAN_POINT ( 'NONE',  ( 3.788215052820487205, 39.19523464621513398, 90.08681233796825438 ) ) ;
#1019 = VECTOR ( 'NONE', #11103, 1000.000000000000000 ) ;
#1020 = APPLICATION_PROTOCOL_DEFINITION ( 'draft international standard', 'automotive_design', 1998, #13207 ) ;
#1021 = CARTESIAN_POINT ( 'NONE',  ( 5.125405977158137283, 37.38264009880134608, 76.06572720930677178 ) ) ;
#1022 = CARTESIAN_POINT ( 'NONE',  ( 5.289916459460165754, 50.82772623642982524, 78.90029747732744170 ) ) ;
#1023 = CARTESIAN_POINT ( 'NONE',  ( 8.868817592801743643, 41.37413345511091478, 75.97198585835440099 ) ) ;
#1024 = EDGE_CURVE ( 'NONE', #5759, #15353, #8350, .T. ) ;
#1025 = EDGE_LOOP ( 'NONE', ( #12403, #18407, #14618, #9974 ) ) ;
#1026 = CARTESIAN_POINT ( 'NONE',  ( 1.555492715512752255, 52.20592956483955760, 75.52862058684291924 ) ) ;
#1027 = AXIS2_PLACEMENT_3D ( 'NONE', #7124, #3723, #1925 ) ;
#1028 = AXIS2_PLACEMENT_3D ( 'NONE', #892, #20351, #15583 ) ;
#1029 = EDGE_CURVE ( 'NONE', #18041, #20573, #10931, .T. ) ;
#1030 = ORIENTED_EDGE ( 'NONE', *, *, #20668, .F. ) ;
#1031 = CARTESIAN_POINT ( 'NONE',  ( 0.6404851603139647409, 52.36132752672286017, 79.54845644658969661 ) ) ;
#1032 = LINE ( 'NONE', #7521, #4797 ) ;
#1033 = CARTESIAN_POINT ( 'NONE',  ( -0.9988176903691428077, 49.83852402762217082, 94.39871380123798872 ) ) ;
#1034 = B_SPLINE_SURFACE_WITH_KNOTS ( 'NONE', 3, 1, ( 
 ( #5879, #17362 ),
 ( #2892, #14065 ),
 ( #18851, #10789 ),
 ( #6178, #2792 ),
 ( #20444, #9293 ),
 ( #1196, #7681 ),
 ( #6071, #9392 ),
 ( #20849, #14374 ),
 ( #15876, #12682 ),
 ( #9183, #17564 ),
 ( #15673, #19162 ),
 ( #12377, #11096 ),
 ( #1093, #9495 ),
 ( #17155, #15981 ),
 ( #7888, #6276 ),
 ( #12778, #10693 ),
 ( #7467, #17256 ),
 ( #11305, #8095 ),
 ( #4779, #14688 ),
 ( #17877, #19469 ),
 ( #7993, #3299 ),
 ( #19677, #10321 ),
 ( #5386, #1610 ),
 ( #4886, #14584 ),
 ( #9807, #11906 ),
 ( #112, #18381 ),
 ( #11, #19570 ) ),
 .UNSPECIFIED., .F., .F., .F.,
 ( 4, 1, 1, 1, 1, 1, 1, 1, 1, 1, 1, 1, 1, 1, 1, 1, 1, 1, 1, 1, 1, 1, 1, 1, 4 ),
 ( 2, 2 ),
 ( 0.000000000000000000, 0.05996724504547770729, 0.1145758167962369900, 0.1640861619357650014, 0.2084987699952417783, 0.2475617630034998851, 0.2815348823686551483, 0.3104252079858747515, 0.3342443525417332362, 0.3765838217147600697, 0.4197110765771541185, 0.4650989620513389933, 0.5135994637417293784, 0.5388633206098475403, 0.5643363709942800233, 0.5903657223275191601, 0.6168353869529757949, 0.6439286963540884479, 0.6717746256502626911, 0.7005904770003053006, 0.7303719928790673999, 0.7923444005162998405, 0.8574606674909915904, 0.9267280696664335071, 1.000000000000000000 ),
 ( 0.000000000000000000, 1.000000000000000000 ),
 .UNSPECIFIED. ) ;
#1035 = VERTEX_POINT ( 'NONE', #2234 ) ;
#1036 = ORIENTED_EDGE ( 'NONE', *, *, #17255, .F. ) ;
#1037 = AXIS2_PLACEMENT_3D ( 'NONE', #12828, #8146, #14742 ) ;
#1038 = EDGE_CURVE ( 'NONE', #476, #10886, #8836, .T. ) ;
#1039 = CARTESIAN_POINT ( 'NONE',  ( 5.593371404305700345, 50.44267676395632805, 79.53335372712579954 ) ) ;
#1040 = EDGE_LOOP ( 'NONE', ( #1291, #9949, #2043, #17962 ) ) ;
#1041 = FACE_OUTER_BOUND ( 'NONE', #16159, .T. ) ;
#1042 = EDGE_CURVE ( 'NONE', #1280, #4828, #6424, .T. ) ;
#1043 = LINE ( 'NONE', #7201, #19684 ) ;
#1044 = CARTESIAN_POINT ( 'NONE',  ( 8.385738467910485383, 39.92631467184355643, 77.08252479744105301 ) ) ;
#1045 = EDGE_CURVE ( 'NONE', #2768, #4997, #19885, .T. ) ;
#1046 = ORIENTED_EDGE ( 'NONE', *, *, #5178, .T. ) ;
#1047 = CARTESIAN_POINT ( 'NONE',  ( -4.578768572918463953, 36.98961260158171882, 78.00876120161012750 ) ) ;
#1048 = CARTESIAN_POINT ( 'NONE',  ( -7.570753287668954279, 40.54925684501983341, 79.32598559883581402 ) ) ;
#1049 = CARTESIAN_POINT ( 'NONE',  ( -7.497174307679370209, 42.44115768106999553, 79.44947929565324785 ) ) ;
#1050 = CARTESIAN_POINT ( 'NONE',  ( -2.416137431568557314, 39.07291177436112406, 92.52371380123797451 ) ) ;
#1051 = AXIS2_PLACEMENT_3D ( 'NONE', #5263, #11780, #2092 ) ;
#1052 = CARTESIAN_POINT ( 'NONE',  ( 24.52215374030650352, 44.16218137147969003, 105.5543387995309956 ) ) ;
#1053 = CARTESIAN_POINT ( 'NONE',  ( 5.712782733624313103, 51.26848743039855094, 75.36064185147203887 ) ) ;
#1054 = ADVANCED_FACE ( 'NONE', ( #8945 ), #19050, .T. ) ;
#1055 = CARTESIAN_POINT ( 'NONE',  ( -3.981178359372548492, 46.76218137147973408, 90.41433880294496817 ) ) ;
#1056 = B_SPLINE_CURVE_WITH_KNOTS ( 'NONE', 3,
 ( #6216, #17218, #7822, #20286, #17599, #14305, #9536, #3027, #4709, #2643, #3237, #12923, #5831, #17709 ),
 .UNSPECIFIED., .F., .F.,
 ( 4, 2, 2, 2, 2, 2, 4 ),
 ( 0.000000000000000000, 0.0001389608718179012755, 0.0002779217436358025510, 0.0003474021795447532158, 0.0004168826154537039349, 0.0004863630513626545997, 0.0005558434872716053188 ),
 .UNSPECIFIED. ) ;
#1057 = VECTOR ( 'NONE', #18086, 1000.000000000000000 ) ;
#1058 = DIRECTION ( 'NONE',  ( 1.540237394707284220E-16, 1.793354297423764243E-16, -1.000000000000000000 ) ) ;
#1059 = VERTEX_POINT ( 'NONE', #3612 ) ;
#1060 = CARTESIAN_POINT ( 'NONE',  ( 6.691294758883309157, 37.75465145915448062, 79.45433879953087342 ) ) ;
#1061 = DIRECTION ( 'NONE',  ( 6.308085367188358095E-15, 0.000000000000000000, 1.000000000000000000 ) ) ;
#1062 = CARTESIAN_POINT ( 'NONE',  ( -4.574316323987747346, 51.33620267474496757, 79.54845644658969661 ) ) ;
#1063 = CARTESIAN_POINT ( 'NONE',  ( -4.567115856812060670, 47.10047254335474065, 90.96121380123797451 ) ) ;
#1064 = CARTESIAN_POINT ( 'NONE',  ( -7.343158166839156564, 42.28655005559638624, 79.49764826322659417 ) ) ;
#1065 = CARTESIAN_POINT ( 'NONE',  ( 5.534247820986439415, 36.92786807952553119, 77.73906448345020692 ) ) ;
#1066 = ORIENTED_EDGE ( 'NONE', *, *, #3550, .T. ) ;
#1067 = CARTESIAN_POINT ( 'NONE',  ( 9.353718648869055130, 42.82741268169404947, 78.44945682776121032 ) ) ;
#1069 = EDGE_CURVE ( 'NONE', #18879, #5725, #3926, .T. ) ;
#1068 = CARTESIAN_POINT ( 'NONE',  ( -3.226449543290886179, 47.76606447477297479, 92.55433879953076826 ) ) ;
#1070 = CARTESIAN_POINT ( 'NONE',  ( 8.940907051378230719, 41.59019013573462331, 76.11674899411023887 ) ) ;
#1071 = CARTESIAN_POINT ( 'NONE',  ( 5.939849532777430774, 51.10076233267274404, 76.96076274685535168 ) ) ;
#1072 = DIRECTION ( 'NONE',  ( -0.000000000000000000, -0.000000000000000000, 1.000000000000000000 ) ) ;
#1073 = B_SPLINE_CURVE_WITH_KNOTS ( 'NONE', 3,
 ( #18568, #4089, #5681, #13993, #15493, #20478, #10506, #12408, #16769, #9006, #16871, #2189, #2401, #20153, #15168, #13778, #5475, #7177, #2609, #582 ),
 .UNSPECIFIED., .F., .F.,
 ( 4, 2, 2, 2, 2, 2, 2, 2, 2, 4 ),
 ( 0.000000000000000000, 0.0002954762126916160841, 0.0005909524253832317345, 0.0008864286380748474933, 0.001181904850766463252, 0.001477381063458079119, 0.001625119169803869489, 0.001772857276149659858, 0.002068333488841280713, 0.002363809701532901784 ),
 .UNSPECIFIED. ) ;
#1074 = VECTOR ( 'NONE', #13384, 1000.000000000000000 ) ;
#1075 = CARTESIAN_POINT ( 'NONE',  ( -4.884656273474450749, 44.39824779480852612, 93.03246379611697137 ) ) ;
#1076 = DIRECTION ( 'NONE',  ( -0.000000000000000000, -0.000000000000000000, 1.000000000000000000 ) ) ;
#1077 = ADVANCED_FACE ( 'NONE', ( #16915 ), #631, .T. ) ;
#1078 = VECTOR ( 'NONE', #6501, 1000.000000000000114 ) ;
#1080 = EDGE_CURVE ( 'NONE', #16996, #20468, #7005, .T. ) ;
#1079 = CARTESIAN_POINT ( 'NONE',  ( -0.9223058776520068891, 52.84282348712751798, 78.54073599580733855 ) ) ;
#1081 = ORIENTED_EDGE ( 'NONE', *, *, #6899, .F. ) ;
#1082 = CARTESIAN_POINT ( 'NONE',  ( -5.955451856753751549, 38.00651308716548726, 78.53742703482498655 ) ) ;
#1083 = CARTESIAN_POINT ( 'NONE',  ( 0.6073277304985209568, 52.36177255988537382, 78.93565971576092011 ) ) ;
#1084 = VERTEX_POINT ( 'NONE', #17022 ) ;
#1085 = CARTESIAN_POINT ( 'NONE',  ( 1.794851674890223459, 52.26306568748834991, 75.67222655803806219 ) ) ;
#1086 = VERTEX_POINT ( 'NONE', #13615 ) ;
#1087 = AXIS2_PLACEMENT_3D ( 'NONE', #9091, #20345, #7269 ) ;
#1088 = LINE ( 'NONE', #4570, #18017 ) ;
#1089 = AXIS2_PLACEMENT_3D ( 'NONE', #10663, #17226, #9366 ) ;
#1090 = CARTESIAN_POINT ( 'NONE',  ( 5.025485839985549319, 41.56218137147963887, 93.53933880294496817 ) ) ;
#1091 = VERTEX_POINT ( 'NONE', #5531 ) ;
#1092 = CARTESIAN_POINT ( 'NONE',  ( 6.660594192354430731, 43.89417127335556046, 93.26683879782399345 ) ) ;
#1093 = CARTESIAN_POINT ( 'NONE',  ( -0.7867047173639660773, 52.21826805272613115, 75.89928829349869943 ) ) ;
#1094 = CARTESIAN_POINT ( 'NONE',  ( 8.946756316568102108, 41.60772075457913388, 78.11862058389174024 ) ) ;
#1095 = DIRECTION ( 'NONE',  ( -1.213411507412056509E-16, 1.000000000000000000, 0.000000000000000000 ) ) ;
#1096 = CARTESIAN_POINT ( 'NONE',  ( -4.409036544953043979, 47.67330854490502645, 72.45432679953087529 ) ) ;
#1097 = CARTESIAN_POINT ( 'NONE',  ( -3.887033836373874784, 37.39267102169923618, 79.51042285023450518 ) ) ;
#1098 = ORIENTED_EDGE ( 'NONE', *, *, #14279, .F. ) ;
#1099 = CARTESIAN_POINT ( 'NONE',  ( 5.838531714063069700, 37.14529820897372758, 77.55803991379978868 ) ) ;
#1100 = CARTESIAN_POINT ( 'NONE',  ( -1.876873622437039257, 39.01745058958429269, 92.71996379782397923 ) ) ;
#1101 = ORIENTED_EDGE ( 'NONE', *, *, #4826, .T. ) ;
#1102 = LINE ( 'NONE', #14466, #8401 ) ;
#1103 = CARTESIAN_POINT ( 'NONE',  ( -3.350035803220276609, 49.20851703305431357, 94.47683880123798872 ) ) ;
#1104 = CARTESIAN_POINT ( 'NONE',  ( -7.320717484398829633, 46.55579181444844750, 79.45433879953087342 ) ) ;
#1105 = CARTESIAN_POINT ( 'NONE',  ( -5.368445182934982185, 36.96218137147968008, 93.55433879953098142 ) ) ;
#1106 = VECTOR ( 'NONE', #16880, 1000.000000000000000 ) ;
#1107 = CARTESIAN_POINT ( 'NONE',  ( -1.876873622437040590, 39.01745058958429269, 95.37621379782397923 ) ) ;
#1108 = CARTESIAN_POINT ( 'NONE',  ( -5.157025508368711542, 37.41674770618861601, 75.39928922905468767 ) ) ;
#1109 = VECTOR ( 'NONE', #10561, 1000.000000000000000 ) ;
#1110 = ORIENTED_EDGE ( 'NONE', *, *, #11608, .F. ) ;
#1111 = CARTESIAN_POINT ( 'NONE',  ( 8.215319998344366326, 41.32401173211437850, 76.31063117824747621 ) ) ;
#1112 = ORIENTED_EDGE ( 'NONE', *, *, #5848, .F. ) ;
#1113 = PLANE ( 'NONE',  #5087 ) ;
#1114 = CARTESIAN_POINT ( 'NONE',  ( 5.611423337425062385, 41.22389019960463230, 94.08621380123797451 ) ) ;
#1115 = CARTESIAN_POINT ( 'NONE',  ( -7.080934810785074696, 41.45028247878327221, 78.59694605312716931 ) ) ;
#1116 = VERTEX_POINT ( 'NONE', #13414 ) ;
#1117 = CARTESIAN_POINT ( 'NONE',  ( 6.198496396448986090, 45.68315280215533392, 92.99246380123798872 ) ) ;
#1118 = CARTESIAN_POINT ( 'NONE',  ( 4.512269934384613990, 47.81844922806527620, 93.81371379611699979 ) ) ;
#1119 = CIRCLE ( 'NONE', #10988, 4.200000000000001954 ) ;
#1120 = CARTESIAN_POINT ( 'NONE',  ( -4.156963686837030103, 37.43267826557348599, 78.61392107264721574 ) ) ;
#1121 = EDGE_CURVE ( 'NONE', #20921, #20010, #12537, .T. ) ;
#1122 = CARTESIAN_POINT ( 'NONE',  ( 5.205681390936892861, 50.88842682295077680, 76.21945306000542075 ) ) ;
#1123 = VECTOR ( 'NONE', #10142, 1000.000000000000227 ) ;
#1124 = EDGE_LOOP ( 'NONE', ( #8653, #3076, #5632, #3231 ) ) ;
#1125 = CARTESIAN_POINT ( 'NONE',  ( 1.868012774839550749, 39.13936707477651566, 93.07058879953099506 ) ) ;
#1126 = CARTESIAN_POINT ( 'NONE',  ( 5.611423337425062385, 41.22389019960463230, 91.58621380123798872 ) ) ;
#1127 = EDGE_LOOP ( 'NONE', ( #16, #17882, #8412, #15082, #6611, #1732 ) ) ;
#1128 = CARTESIAN_POINT ( 'NONE',  ( -5.014338679419717337, 43.53652754521196044, 92.45433879953098710 ) ) ;
#1129 = LINE ( 'NONE', #14304, #11229 ) ;
#1130 = CARTESIAN_POINT ( 'NONE',  ( 6.660594192354429843, 43.89417127335556046, 94.51683879782399345 ) ) ;
#1131 = CARTESIAN_POINT ( 'NONE',  ( 0.000000000000000000, 0.000000000000000000, 0.000000000000000000 ) ) ;
#1132 = CARTESIAN_POINT ( 'NONE',  ( 5.464930624430781592, 36.87833654873140432, 76.10043865634602867 ) ) ;
#1133 = CARTESIAN_POINT ( 'NONE',  ( 8.792356959002002981, 41.14497608504091630, 76.18655208513948196 ) ) ;
#1134 = DIRECTION ( 'NONE',  ( 0.000000000000000000, 0.000000000000000000, 1.000000000000000000 ) ) ;
#1135 = VERTEX_POINT ( 'NONE', #5409 ) ;
#1136 = ADVANCED_FACE ( 'NONE', ( #6910 ), #5733, .T. ) ;
#1137 = CARTESIAN_POINT ( 'NONE',  ( 2.114670974380917112, 52.20152023876698166, 76.45922371407752394 ) ) ;
#1138 = ORIENTED_EDGE ( 'NONE', *, *, #17818, .F. ) ;
#1139 = CARTESIAN_POINT ( 'NONE',  ( 6.695638642021790155, 50.54249136271632636, 75.66183449524544358 ) ) ;
#1140 = CARTESIAN_POINT ( 'NONE',  ( 5.495239211387634271, 37.64690938752282534, 77.40928489470421425 ) ) ;
#1141 = CARTESIAN_POINT ( 'NONE',  ( 4.394343283833276992, 39.11584570990505938, 91.50808880123798872 ) ) ;
#1142 = CARTESIAN_POINT ( 'NONE',  ( -4.138842527380969472, 50.91175009559962916, 75.36205588254068743 ) ) ;
#1143 = ORIENTED_EDGE ( 'NONE', *, *, #16420, .T. ) ;
#1144 = CARTESIAN_POINT ( 'NONE',  ( -4.812088799398940075, 42.22067586467031930, 93.81371379782397923 ) ) ;
#1145 = VERTEX_POINT ( 'NONE', #9758 ) ;
#1146 = CARTESIAN_POINT ( 'NONE',  ( -3.580888326837075475, 36.25251866086962593, 75.96390267329995538 ) ) ;
#1147 = CARTESIAN_POINT ( 'NONE',  ( -4.909077168075741682, 50.30854671200530959, 75.47180400867900119 ) ) ;
#1148 = ORIENTED_EDGE ( 'NONE', *, *, #11269, .T. ) ;
#1149 = CARTESIAN_POINT ( 'NONE',  ( 4.174832730680089199, 51.49049413994026025, 78.81874598975664981 ) ) ;
#1150 = PLANE ( 'NONE',  #7800 ) ;
#1151 = CARTESIAN_POINT ( 'NONE',  ( 0.7582201636353291807, 49.56899138526064519, 91.78246379953097289 ) ) ;
#1152 = VECTOR ( 'NONE', #18705, 1000.000000000000114 ) ;
#1153 = EDGE_CURVE ( 'NONE', #14867, #8763, #4842, .T. ) ;
#1154 = ORIENTED_EDGE ( 'NONE', *, *, #10571, .F. ) ;
#1155 = CARTESIAN_POINT ( 'NONE',  ( 6.520305832453487049, 49.75344699685330596, 76.44686420531779447 ) ) ;
#1156 = CARTESIAN_POINT ( 'NONE',  ( -6.705005553477274560, 40.29739814665693132, 78.50801527011910252 ) ) ;
#1157 = CARTESIAN_POINT ( 'NONE',  ( -5.509791672390228712, 38.60739634041024715, 78.62262977491066351 ) ) ;
#1158 = CARTESIAN_POINT ( 'NONE',  ( 5.568489401881125289, 48.03437091500646261, 91.82058880123797451 ) ) ;
#1159 = DIRECTION ( 'NONE',  ( 1.000000000000000000, 0.000000000000000000, 0.000000000000000000 ) ) ;
#1160 = CARTESIAN_POINT ( 'NONE',  ( 5.008928291858447679, 51.78839635354462700, 75.50506468444432073 ) ) ;
#1161 = CARTESIAN_POINT ( 'NONE',  ( 6.102441102155617969, 43.42752260303680600, 93.61746380294498238 ) ) ;
#1162 = EDGE_CURVE ( 'NONE', #19108, #5214, #13598, .T. ) ;
#1163 = CARTESIAN_POINT ( 'NONE',  ( 9.026838159693451047, 41.84773111872319618, 78.13669174070733447 ) ) ;
#1164 = CARTESIAN_POINT ( 'NONE',  ( 8.946998292058729874, 41.60844597047518789, 78.80177617112552468 ) ) ;
#1165 =( BOUNDED_SURFACE ( )  B_SPLINE_SURFACE ( 1, 2, ( 
 ( #13582, #4001, #5602, #2308, #18482, #3897, #8919, #3793, #13478, #19951, #8804, #10419, #714, #1997, #7195, #18375, #16989, #6975, #499, #3586, #12107, #2420, #10314, #18585, #396, #2203, #15407, #8704, #15184, #5174, #13385, #11694, #19855, #5275, #11790, #18266, #16683, #2107, #8607, #15085, #7729, #922, #7306, #9439, #4524, #19004, #10939, #12423, #5816, #6125, #18902, #7410, #20494, #2527, #821, #10841, #20592, #15723, #13795, #1237, #2935, #1141, #14211, #7522, #11041, #17203, #6020, #13899, #20383, #18690, #12322, #17306, #5701, #20270, #5926, #15614, #12208, #4106, #12628, #10636, #18802 ),
 ( #4314, #4215, #15826, #9340, #2626, #7629, #19112, #20687, #17411, #14110, #12520, #17104, #2732, #14011, #9235, #2836, #4424, #17513, #9023, #15509, #10740, #9127, #1033, #11502, #11941, #11710, #16592, #3397, #5092, #16281, #201, #14781, #10012, #17867, #14995, #6477, #14677, #16177, #8402, #8085, #3290, #16489, #13191, #8512, #1601, #14880, #9796, #303, #11609, #6795, #8299, #1817, #1909, #19561, #12982, #19460, #6685, #16390, #9909, #4982, #19665, #4875, #18084, #3503, #11397, #13300, #19773, #5192, #18185, #102, #3602, #8187, #10110, #2013, #6582, #13087, #16226, #1650, #3243, #17918, #3340 ) ),
 .UNSPECIFIED., .F., .F., .F. ) 
 B_SPLINE_SURFACE_WITH_KNOTS ( ( 2, 2 ),
 ( 3, 2, 2, 2, 2, 2, 2, 2, 2, 2, 2, 2, 2, 2, 2, 2, 2, 2, 2, 2, 2, 2, 2, 2, 2, 2, 2, 2, 2, 2, 2, 2, 2, 2, 2, 2, 2, 2, 2, 2, 3 ),
 ( 0.000000000000000000, 1.000000000000000000 ),
 ( 0.000000000000000000, 0.02500000000000000139, 0.05000000000000000278, 0.07499999999999999722, 0.1000000000000000056, 0.1250000000000000000, 0.1499999999999999944, 0.1749999999999999889, 0.2000000000000000111, 0.2250000000000000056, 0.2500000000000000000, 0.2750000000000000222, 0.2999999999999999889, 0.3250000000000000111, 0.3499999999999999778, 0.3750000000000000000, 0.4000000000000000222, 0.4249999999999999889, 0.4500000000000000111, 0.4749999999999999778, 0.5000000000000000000, 0.5250000000000000222, 0.5500000000000000444, 0.5749999999999999556, 0.5999999999999999778, 0.6250000000000000000, 0.6500000000000000222, 0.6750000000000000444, 0.6999999999999999556, 0.7249999999999999778, 0.7500000000000000000, 0.7750000000000000222, 0.8000000000000000444, 0.8249999999999999556, 0.8499999999999999778, 0.8750000000000000000, 0.9000000000000000222, 0.9250000000000000444, 0.9499999999999999556, 0.9600309411673831894, 0.9696312505790569691 ),
 .UNSPECIFIED. ) 
 GEOMETRIC_REPRESENTATION_ITEM ( )  RATIONAL_B_SPLINE_SURFACE ( (
 ( 1.000000000000000000, 0.9238795325112867385, 1.000000000000000000, 0.9238795325112867385, 1.000000000000000000, 0.9238795325112867385, 1.000000000000000000, 0.9238795325112867385, 1.000000000000000000, 0.9238795325112867385, 1.000000000000000000, 0.9238795325112867385, 1.000000000000000000, 0.9238795325112867385, 1.000000000000000000, 0.9238795325112867385, 1.000000000000000000, 0.9238795325112867385, 1.000000000000000000, 0.9238795325112867385, 1.000000000000000000, 0.9238795325112867385, 1.000000000000000000, 0.9238795325112867385, 1.000000000000000000, 0.9238795325112867385, 1.000000000000000000, 0.9238795325112867385, 1.000000000000000000, 0.9238795325112867385, 1.000000000000000000, 0.9238795325112867385, 1.000000000000000000, 0.9238795325112867385, 1.000000000000000000, 0.9238795325112867385, 1.000000000000000000, 0.9238795325112867385, 1.000000000000000000, 0.9238795325112867385, 1.000000000000000000, 0.9238795325112867385, 1.000000000000000000, 0.9238795325112867385, 1.000000000000000000, 0.9238795325112867385, 1.000000000000000000, 0.9238795325112867385, 1.000000000000000000, 0.9238795325112867385, 1.000000000000000000, 0.9238795325112867385, 1.000000000000000000, 0.9238795325112867385, 1.000000000000000000, 0.9238795325112867385, 1.000000000000000000, 0.9238795325112867385, 1.000000000000000000, 0.9238795325112867385, 1.000000000000000000, 0.9238795325112867385, 1.000000000000000000, 0.9238795325112867385, 1.000000000000000000, 0.9238795325112867385, 1.000000000000000000, 0.9238795325112867385, 1.000000000000000000, 0.9238795325112867385, 1.000000000000000000, 0.9238795325112867385, 1.000000000000000000, 0.9238795325112867385, 1.000000000000000000, 0.9238795325112867385, 1.000000000000000000, 0.9694576027594803413, 0.9634247247054007479, 0.9634247247054007479, 0.9634247247054007479),
 ( 1.000000000000000000, 0.9238795325112867385, 1.000000000000000000, 0.9238795325112867385, 1.000000000000000000, 0.9238795325112867385, 1.000000000000000000, 0.9238795325112867385, 1.000000000000000000, 0.9238795325112867385, 1.000000000000000000, 0.9238795325112867385, 1.000000000000000000, 0.9238795325112867385, 1.000000000000000000, 0.9238795325112867385, 1.000000000000000000, 0.9238795325112867385, 1.000000000000000000, 0.9238795325112867385, 1.000000000000000000, 0.9238795325112867385, 1.000000000000000000, 0.9238795325112867385, 1.000000000000000000, 0.9238795325112867385, 1.000000000000000000, 0.9238795325112867385, 1.000000000000000000, 0.9238795325112867385, 1.000000000000000000, 0.9238795325112867385, 1.000000000000000000, 0.9238795325112867385, 1.000000000000000000, 0.9238795325112867385, 1.000000000000000000, 0.9238795325112867385, 1.000000000000000000, 0.9238795325112867385, 1.000000000000000000, 0.9238795325112867385, 1.000000000000000000, 0.9238795325112867385, 1.000000000000000000, 0.9238795325112867385, 1.000000000000000000, 0.9238795325112867385, 1.000000000000000000, 0.9238795325112867385, 1.000000000000000000, 0.9238795325112867385, 1.000000000000000000, 0.9238795325112867385, 1.000000000000000000, 0.9238795325112867385, 1.000000000000000000, 0.9238795325112867385, 1.000000000000000000, 0.9238795325112867385, 1.000000000000000000, 0.9238795325112867385, 1.000000000000000000, 0.9238795325112867385, 1.000000000000000000, 0.9238795325112867385, 1.000000000000000000, 0.9238795325112867385, 1.000000000000000000, 0.9238795325112867385, 1.000000000000000000, 0.9238795325112867385, 1.000000000000000000, 0.9238795325112867385, 1.000000000000000000, 0.9238795325112867385, 1.000000000000000000, 0.9694576027594803413, 0.9634247247054007479, 0.9634247247054007479, 0.9634247247054007479) ) ) 
 REPRESENTATION_ITEM ( '' )  SURFACE ( )  );
#1166 = CARTESIAN_POINT ( 'NONE',  ( -4.006646489220814011, 48.09791109810387155, 82.45433879953087342 ) ) ;
#1167 = AXIS2_PLACEMENT_3D ( 'NONE', #223, #8004, #1838 ) ;
#1168 = PLANE ( 'NONE',  #1012 ) ;
#1169 = CARTESIAN_POINT ( 'NONE',  ( 27.03948732994508930, 36.35905713404685713, 76.90433879953101837 ) ) ;
#1170 = DIRECTION ( 'NONE',  ( 0.5813877811927011807, -0.8136266022444372803, -5.636455622144619183E-17 ) ) ;
#1171 = CARTESIAN_POINT ( 'NONE',  ( 5.561379608955574483, 51.38032281970146897, 76.39036821129558064 ) ) ;
#1172 = CARTESIAN_POINT ( 'NONE',  ( 5.184346195580738836, 46.85389944054460898, 94.68362681315549878 ) ) ;
#1173 = LINE ( 'NONE', #7333, #12306 ) ;
#1174 = VERTEX_POINT ( 'NONE', #21000 ) ;
#1175 = CARTESIAN_POINT ( 'NONE',  ( 8.215457551141771120, 41.32437277815750321, 78.72120140517411357 ) ) ;
#1176 = CARTESIAN_POINT ( 'NONE',  ( -3.964734524320789877, 36.53605038468285215, 79.39152984579853012 ) ) ;
#1177 = CARTESIAN_POINT ( 'NONE',  ( 0.3821786226492924210, 35.36301154328572949, 78.57639762306027365 ) ) ;
#1178 = DIRECTION ( 'NONE',  ( 0.6080936526121289987, 0.7938652969193448206, 2.360290325043240801E-16 ) ) ;
#1179 = CARTESIAN_POINT ( 'NONE',  ( 0.5221537403065097394, 44.16218137147969003, 92.55433879953098142 ) ) ;
#1180 = FACE_OUTER_BOUND ( 'NONE', #5813, .T. ) ;
#1181 = LINE ( 'NONE', #17652, #14883 ) ;
#1182 = CARTESIAN_POINT ( 'NONE',  ( 6.198496396448986090, 45.68315280215533392, 92.83621380123798872 ) ) ;
#1183 = CARTESIAN_POINT ( 'NONE',  ( -3.350035803220276609, 49.20851703305431357, 90.72683880123797451 ) ) ;
#1184 = EDGE_CURVE ( 'NONE', #20695, #4844, #6435, .T. ) ;
#1185 = CARTESIAN_POINT ( 'NONE',  ( 0.5221537403065061866, 44.16218137147969713, 74.55433879953100984 ) ) ;
#1186 = EDGE_CURVE ( 'NONE', #15454, #9664, #12945, .T. ) ;
#1187 = DIRECTION ( 'NONE',  ( -0.3165065846431824870, -0.9485903129789529098, 0.000000000000000000 ) ) ;
#1188 = B_SPLINE_CURVE_WITH_KNOTS ( 'NONE', 3,
 ( #283, #6355, #16164, #4649, #13174, #11170, #19334, #19648, #86, #8383, #4753, #11486, #3183, #4964, #13073, #5073, #19548, #11591, #3486, #8068 ),
 .UNSPECIFIED., .F., .F.,
 ( 4, 2, 2, 2, 2, 2, 2, 2, 2, 4 ),
 ( 0.000000000000000000, 0.0002953950361844887278, 0.0005907900723689777809, 0.0008861851085534668340, 0.001181580144737955779, 0.001476975180922444940, 0.001624672699014688328, 0.001772370217106931283, 0.002067765253291418710, 0.002363160289475906353 ),
 .UNSPECIFIED. ) ;
#1189 = ORIENTED_EDGE ( 'NONE', *, *, #1153, .T. ) ;
#1190 = CARTESIAN_POINT ( 'NONE',  ( -10.17784625969349754, 36.96218137147968008, 80.55433879953099563 ) ) ;
#1191 = EDGE_CURVE ( 'NONE', #3376, #9436, #6232, .T. ) ;
#1192 = CARTESIAN_POINT ( 'NONE',  ( 1.868012774839550749, 39.13936707477651566, 93.38308880294498238 ) ) ;
#1193 = ORIENTED_EDGE ( 'NONE', *, *, #18475, .F. ) ;
#1194 = CARTESIAN_POINT ( 'NONE',  ( -1.876873622437039701, 39.01745058958429269, 94.12621379782397923 ) ) ;
#1195 = ADVANCED_FACE ( 'NONE', ( #20899 ), #19423, .F. ) ;
#1196 = CARTESIAN_POINT ( 'NONE',  ( -0.9375027607463610746, 52.21945715071739613, 76.61976384666378692 ) ) ;
#1197 = CYLINDRICAL_SURFACE ( 'NONE', #14231, 5.199999999999999289 ) ;
#1198 = LINE ( 'NONE', #16086, #19909 ) ;
#1199 = FACE_BOUND ( 'NONE', #14600, .T. ) ;
#1200 = LINE ( 'NONE', #13102, #414 ) ;
#1201 = ORIENTED_EDGE ( 'NONE', *, *, #15742, .F. ) ;
#1202 = CARTESIAN_POINT ( 'NONE',  ( 8.887668352622405621, 41.43063037816333605, 75.36022115247205022 ) ) ;
#1203 = VERTEX_POINT ( 'NONE', #17616 ) ;
#1204 = CARTESIAN_POINT ( 'NONE',  ( -0.9988176903691428077, 49.83852402762217082, 95.64871380123798872 ) ) ;
#1205 = CARTESIAN_POINT ( 'NONE',  ( 11.22215374030650281, 42.76218137147968434, 64.80574467885102763 ) ) ;
#1206 = CARTESIAN_POINT ( 'NONE',  ( 11.22215374030650281, 42.96218137147968008, 74.20433879953100131 ) ) ;
#1207 = LINE ( 'NONE', #4489, #17796 ) ;
#1208 = DIRECTION ( 'NONE',  ( 0.3165065846431826535, 0.9485903129789529098, 2.188653791613874008E-16 ) ) ;
#1209 = EDGE_LOOP ( 'NONE', ( #19382, #9526, #13523, #2331, #4212, #956 ) ) ;
#1210 = CARTESIAN_POINT ( 'NONE',  ( 8.227529334238381509, 41.35732131334246731, 76.09516292429817952 ) ) ;
#1211 = VERTEX_POINT ( 'NONE', #10668 ) ;
#1212 = CARTESIAN_POINT ( 'NONE',  ( -3.061196554867672948, 51.49764708062921414, 75.88277413867518817 ) ) ;
#1213 = EDGE_CURVE ( 'NONE', #11255, #20468, #7735, .T. ) ;
#1214 = CARTESIAN_POINT ( 'NONE',  ( -5.154188915835984375, 42.64120994080404614, 96.11746380123797451 ) ) ;
#1215 = CARTESIAN_POINT ( 'NONE',  ( -7.081455809225041698, 41.45193003946861410, 78.55785233681892521 ) ) ;
#1216 = ORIENTED_EDGE ( 'NONE', *, *, #418, .T. ) ;
#1217 = CARTESIAN_POINT ( 'NONE',  ( 0.7901638384306272078, 50.30062182352762079, 94.67308879782399345 ) ) ;
#1218 = DIRECTION ( 'NONE',  ( -1.540237394707284467E-16, -1.793354297423764243E-16, 1.000000000000000000 ) ) ;
#1219 = ORIENTED_EDGE ( 'NONE', *, *, #3797, .F. ) ;
#1220 = DIRECTION ( 'NONE',  ( -1.540237394707284220E-16, -1.793354297423764243E-16, 1.000000000000000000 ) ) ;
#1221 = CARTESIAN_POINT ( 'NONE',  ( 5.619974078175711263, 51.33704144561774996, 76.01203914421944319 ) ) ;
#1222 = ORIENTED_EDGE ( 'NONE', *, *, #654, .T. ) ;
#1223 = CARTESIAN_POINT ( 'NONE',  ( 0.5221537403065009686, 44.16218137147968292, 79.45433879953087342 ) ) ;
#1224 = CARTESIAN_POINT ( 'NONE',  ( 0.7188031343443799237, 52.96453286013366579, 78.90093525964157095 ) ) ;
#1225 = ORIENTED_EDGE ( 'NONE', *, *, #9336, .F. ) ;
#1226 = DIRECTION ( 'NONE',  ( -1.540237394707283727E-16, -1.793354297423763257E-16, 1.000000000000000000 ) ) ;
#1227 = CARTESIAN_POINT ( 'NONE',  ( 0.5221537403065013017, 44.16218137147968292, 76.86610350541323555 ) ) ;
#1228 = CARTESIAN_POINT ( 'NONE',  ( -4.007890887056452911, 40.01116025973682611, 95.29808879782397923 ) ) ;
#1229 = CARTESIAN_POINT ( 'NONE',  ( 5.102094394548418954, 37.36598249535994398, 76.14053225265315916 ) ) ;
#1230 = CARTESIAN_POINT ( 'NONE',  ( 5.427780505986065762, 36.85179043424346190, 76.70433879953087342 ) ) ;
#1231 = CARTESIAN_POINT ( 'NONE',  ( -3.798187483714133172, 36.41302879471073339, 77.61986069475027250 ) ) ;
#1232 = ORIENTED_EDGE ( 'NONE', *, *, #4583, .F. ) ;
#1233 = CARTESIAN_POINT ( 'NONE',  ( 2.120636086428073774, 52.95414912482170422, 78.26636343789274974 ) ) ;
#1234 = ORIENTED_EDGE ( 'NONE', *, *, #3605, .T. ) ;
#1235 = LINE ( 'NONE', #9547, #13257 ) ;
#1236 = CARTESIAN_POINT ( 'NONE',  ( 5.377879434019748217, 37.56304838743142227, 77.74321050730907245 ) ) ;
#1237 = CARTESIAN_POINT ( 'NONE',  ( 6.828503391016846891, 43.33193468930419101, 91.66433880123796030 ) ) ;
#1238 = CARTESIAN_POINT ( 'NONE',  ( -2.917199766949189588, 51.60602765227618960, 76.69845644658968808 ) ) ;
#1239 = ORIENTED_EDGE ( 'NONE', *, *, #4663, .T. ) ;
#1240 = ORIENTED_EDGE ( 'NONE', *, *, #783, .F. ) ;
#1241 = CARTESIAN_POINT ( 'NONE',  ( -4.067689360272797039, 37.53693192171343185, 75.36838243422435824 ) ) ;
#1242 = CARTESIAN_POINT ( 'NONE',  ( -6.752712905682232147, 40.37832409722801685, 78.03977571741488362 ) ) ;
#1243 = APPLICATION_CONTEXT ( 'automotive_design' ) ;
#1244 = ORIENTED_EDGE ( 'NONE', *, *, #18450, .F. ) ;
#1245 = CARTESIAN_POINT ( 'NONE',  ( 4.639020460657009792, 52.06163236765677738, 78.92424046551381878 ) ) ;
#1246 = CARTESIAN_POINT ( 'NONE',  ( 8.806278593017598411, 41.18670010535765869, 77.44807837618913027 ) ) ;
#1247 = CARTESIAN_POINT ( 'NONE',  ( 8.387827792284632267, 39.93257650953714943, 76.58175473889373563 ) ) ;
#1248 = VECTOR ( 'NONE', #173, 1000.000000000000000 ) ;
#1249 = ORIENTED_EDGE ( 'NONE', *, *, #13683, .T. ) ;
#1250 = CARTESIAN_POINT ( 'NONE',  ( 6.508108282020931057, 49.76650363545953581, 76.25652011681395948 ) ) ;
#1251 = CARTESIAN_POINT ( 'NONE',  ( 5.761154613439540384, 51.23275707131721646, 77.94923276678728996 ) ) ;
#1252 = FACE_OUTER_BOUND ( 'NONE', #18310, .T. ) ;
#1253 = CARTESIAN_POINT ( 'NONE',  ( 6.828503391016846891, 43.33193468930419101, 90.41433880123798872 ) ) ;
#1254 = ADVANCED_FACE ( 'NONE', ( #3048 ), #18871, .F. ) ;
#1255 =( LENGTH_UNIT ( ) NAMED_UNIT ( * ) SI_UNIT ( .MILLI., .METRE. ) );
#1256 = CARTESIAN_POINT ( 'NONE',  ( 6.348731048540022570, 38.39225852662888627, 77.99342907322302665 ) ) ;
#1257 = DIRECTION ( 'NONE',  ( -1.540237394707284220E-16, -1.793354297423764243E-16, 1.000000000000000000 ) ) ;
#1258 = CARTESIAN_POINT ( 'NONE',  ( 8.527988662190095326, 48.03182059810101379, 79.44551527011911674 ) ) ;
#1259 = EDGE_CURVE ( 'NONE', #3817, #16083, #10291, .T. ) ;
#1260 = CARTESIAN_POINT ( 'NONE',  ( -0.9435164075001931661, 52.21748252032886484, 77.82884852524264829 ) ) ;
#1261 = VECTOR ( 'NONE', #7367, 1000.000000000000227 ) ;
#1262 = CARTESIAN_POINT ( 'NONE',  ( 7.680032241523796266, 40.16158449578585277, 72.45433879953087342 ) ) ;
#1263 = CARTESIAN_POINT ( 'NONE',  ( 8.604143167063659448, 40.58088741054138637, 79.41216397796385706 ) ) ;
#1264 = PLANE ( 'NONE',  #1089 ) ;
#1265 = ORIENTED_EDGE ( 'NONE', *, *, #7512, .T. ) ;
#1266 = CARTESIAN_POINT ( 'NONE',  ( -8.305235601612645624, 42.87665183533326996, 78.69093640348562246 ) ) ;
#1267 = CARTESIAN_POINT ( 'NONE',  ( 5.317402881116432667, 37.51983405691463958, 75.97247164366282846 ) ) ;
#1268 = VERTEX_POINT ( 'NONE', #67 ) ;
#1269 = CARTESIAN_POINT ( 'NONE',  ( -4.535380886826608560, 37.70757786157348335, 78.71874188495704061 ) ) ;
#1270 = CARTESIAN_POINT ( 'NONE',  ( -4.811608766808348037, 37.16160227343304712, 79.54845644658969661 ) ) ;
#1271 = CARTESIAN_POINT ( 'NONE',  ( -4.753421688333184569, 37.11862182248194131, 78.93508260432024315 ) ) ;
#1272 = CARTESIAN_POINT ( 'NONE',  ( -1.077846259693497899, 47.82824192744436687, 85.55433879953100984 ) ) ;
#1273 = CARTESIAN_POINT ( 'NONE',  ( 5.605612954821764582, 51.34764942893797013, 78.13212606300182017 ) ) ;
#1274 = AXIS2_PLACEMENT_3D ( 'NONE', #5713, #8813, #15307 ) ;
#1275 = EDGE_CURVE ( 'NONE', #7517, #13896, #11465, .T. ) ;
#1276 = CARTESIAN_POINT ( 'NONE',  ( 8.582646700885783630, 42.88087918820886557, 77.82525376769920911 ) ) ;
#1277 = FACE_OUTER_BOUND ( 'NONE', #14353, .T. ) ;
#1278 = DIRECTION ( 'NONE',  ( -1.000000000000000000, 1.193617070626243484E-16, 0.000000000000000000 ) ) ;
#1279 =( BOUNDED_CURVE ( )  B_SPLINE_CURVE ( 3, ( #1312, #9509, #3215, #7901 ),
 .UNSPECIFIED., .F., .F. ) 
 B_SPLINE_CURVE_WITH_KNOTS ( ( 4, 4 ),
 ( 4.605568300160951090, 4.721714797055254209 ),
 .UNSPECIFIED. ) 
 CURVE ( )  GEOMETRIC_REPRESENTATION_ITEM ( )  RATIONAL_B_SPLINE_CURVE ( ( 1.000000000000000000, 0.9988761485075002833, 0.9988761485075002833, 1.000000000000000000 ) ) 
 REPRESENTATION_ITEM ( '' )  );
#1280 = VERTEX_POINT ( 'NONE', #16349 ) ;
#1281 = CARTESIAN_POINT ( 'NONE',  ( -2.416137431568557314, 39.07291177436112406, 92.36746380123797451 ) ) ;
#1282 = CIRCLE ( 'NONE', #5337, 4.000000000000003553 ) ;
#1283 = EDGE_CURVE ( 'NONE', #6065, #4311, #16767, .T. ) ;
#1284 = CARTESIAN_POINT ( 'NONE',  ( 0.7995893671964704463, 52.35749147831580075, 78.82132991813820411 ) ) ;
#1285 = CARTESIAN_POINT ( 'NONE',  ( -3.473388836350903119, 37.00066556884812030, 77.65937392779746062 ) ) ;
#1286 = EDGE_CURVE ( 'NONE', #6210, #10787, #11772, .T. ) ;
#1287 = VERTEX_POINT ( 'NONE', #18043 ) ;
#1288 = AXIS2_PLACEMENT_3D ( 'NONE', #16842, #4059, #3469 ) ;
#1289 = DIRECTION ( 'NONE',  ( 0.9999689119394086223, -0.007885122365274166434, 1.526048693634355610E-16 ) ) ;
#1290 = CARTESIAN_POINT ( 'NONE',  ( -0.2125050281363792815, 38.58189400963055959, 93.30496380294501080 ) ) ;
#1291 = ORIENTED_EDGE ( 'NONE', *, *, #9499, .F. ) ;
#1292 = CARTESIAN_POINT ( 'NONE',  ( 5.901851037876958195, 51.12883029018298231, 78.62249727093715990 ) ) ;
#1293 = CARTESIAN_POINT ( 'NONE',  ( -4.500660556396669065, 42.81632233694663370, 94.00808879953098085 ) ) ;
#1294 = CARTESIAN_POINT ( 'NONE',  ( 4.719835101441633540, 52.00193784792148222, 79.11209812681292419 ) ) ;
#1295 = DIRECTION ( 'NONE',  ( 1.000000000000000000, 0.000000000000000000, 0.000000000000000000 ) ) ;
#1296 = CARTESIAN_POINT ( 'NONE',  ( 0.7200154223361650008, 52.35315281306618829, 75.99814205791308552 ) ) ;
#1297 = DIRECTION ( 'NONE',  ( -0.007885122365275663500, -0.9999689119394085113, -1.805443505845543142E-16 ) ) ;
#1298 = EDGE_CURVE ( 'NONE', #13246, #3817, #8302, .T. ) ;
#1299 = ORIENTED_EDGE ( 'NONE', *, *, #11045, .F. ) ;
#1300 = EDGE_CURVE ( 'NONE', #13048, #19006, #5153, .T. ) ;
#1301 = CARTESIAN_POINT ( 'NONE',  ( 8.868817592801743643, 41.37413345511091478, 75.97198585835440099 ) ) ;
#1302 = EDGE_CURVE ( 'NONE', #11635, #15007, #5361, .T. ) ;
#1303 = VECTOR ( 'NONE', #3193, 1000.000000000000227 ) ;
#1304 = ORIENTED_EDGE ( 'NONE', *, *, #14130, .F. ) ;
#1305 = EDGE_CURVE ( 'NONE', #12967, #3115, #17935, .T. ) ;
#1306 = CARTESIAN_POINT ( 'NONE',  ( -2.083470957239373256, 47.45622447009557021, 82.45433879953087342 ) ) ;
#1307 = CARTESIAN_POINT ( 'NONE',  ( -0.02883801100815608018, 35.36625256049322275, 79.45433879953087342 ) ) ;
#1308 = DIRECTION ( 'NONE',  ( 1.540237394707284220E-16, 1.793354297423764243E-16, -1.000000000000000000 ) ) ;
#1309 = PRODUCT_RELATED_PRODUCT_CATEGORY ( 'part', '', ( #19896 ) ) ;
#1310 = B_SPLINE_CURVE_WITH_KNOTS ( 'NONE', 3,
 ( #11866, #18343, #5039, #18033, #3456, #9967 ),
 .UNSPECIFIED., .F., .F.,
 ( 4, 2, 4 ),
 ( 0.000000000000000000, 0.001391361808504451786, 0.002782723617008903572 ),
 .UNSPECIFIED. ) ;
#1311 = CARTESIAN_POINT ( 'NONE',  ( 4.155789158466160593, 39.80095668645486029, 95.60097199408900792 ) ) ;
#1312 = CARTESIAN_POINT ( 'NONE',  ( 8.559588968570775336, 45.78687671259945802, 75.44992703482499508 ) ) ;
#1313 = EDGE_CURVE ( 'NONE', #10052, #4005, #8365, .T. ) ;
#1314 = EDGE_LOOP ( 'NONE', ( #18437, #9465, #7349, #17556 ) ) ;
#1315 = CARTESIAN_POINT ( 'NONE',  ( 4.623413712694776301, 52.07316044369832042, 78.06776350345396054 ) ) ;
#1316 = CIRCLE ( 'NONE', #3006, 4.200000000000000178 ) ;
#1317 = EDGE_LOOP ( 'NONE', ( #15615, #5320, #19697, #944 ) ) ;
#1318 = CARTESIAN_POINT ( 'NONE',  ( -2.961117163336547620, 51.56916014967697492, 76.13050287850805375 ) ) ;
#1319 = CARTESIAN_POINT ( 'NONE',  ( -2.416137431568557314, 39.07291177436112406, 92.52371380123797451 ) ) ;
#1320 = CARTESIAN_POINT ( 'NONE',  ( -7.150160440251022820, 41.66919565927783253, 78.04033446252860529 ) ) ;
#1321 = EDGE_LOOP ( 'NONE', ( #12087, #10715, #13866, #4940 ) ) ;
#1322 = CARTESIAN_POINT ( 'NONE',  ( -5.352023103366428280, 49.86053488430150793, 78.79017217825926878 ) ) ;
#1323 = CARTESIAN_POINT ( 'NONE',  ( -4.498303996637021740, 46.81144376258747997, 95.05433879953096721 ) ) ;
#1324 = CARTESIAN_POINT ( 'NONE',  ( 6.663926478743484871, 37.73509508818325031, 78.14418354478426920 ) ) ;
#1325 = CARTESIAN_POINT ( 'NONE',  ( 5.363666972247387754, 50.77172923808412008, 75.97249762499970416 ) ) ;
#1326 = EDGE_LOOP ( 'NONE', ( #5467, #17768, #6729, #1865 ) ) ;
#1327 = DIRECTION ( 'NONE',  ( -1.402518428993831676E-16, 1.000000000000000000, 0.000000000000000000 ) ) ;
#1328 = CARTESIAN_POINT ( 'NONE',  ( -2.416137431568557314, 39.07291177436112406, 91.27371380123798872 ) ) ;
#1329 = VERTEX_POINT ( 'NONE', #1780 ) ;
#1330 = DIRECTION ( 'NONE',  ( 0.3165065846431826535, 0.9485903129789529098, 2.188653791613874008E-16 ) ) ;
#1331 = DIRECTION ( 'NONE',  ( -0.3015081906286226077, 0.9534635866061452747, 1.245503830460468341E-16 ) ) ;
#1332 = EDGE_CURVE ( 'NONE', #16083, #4532, #2463, .T. ) ;
#1333 = VECTOR ( 'NONE', #1915, 1000.000000000000114 ) ;
#1334 = DIRECTION ( 'NONE',  ( -0.5813877811927011807, 0.8136266022444372803, 5.636455622144619183E-17 ) ) ;
#1335 = CARTESIAN_POINT ( 'NONE',  ( -4.622577041588896485, 46.56120873422322859, 92.56371379782397923 ) ) ;
#1336 = CARTESIAN_POINT ( 'NONE',  ( 5.655950003444441876, 37.76811099897118851, 78.37198585835440667 ) ) ;
#1337 = EDGE_CURVE ( 'NONE', #16241, #9835, #19835, .T. ) ;
#1338 = DIRECTION ( 'NONE',  ( 1.540237394707284220E-16, 1.793354297423764243E-16, -1.000000000000000000 ) ) ;
#1339 = CARTESIAN_POINT ( 'NONE',  ( 5.543757954317092285, 50.63870328413648991, 76.06909773771320715 ) ) ;
#1340 = ORIENTED_EDGE ( 'NONE', *, *, #12820, .F. ) ;
#1341 = CARTESIAN_POINT ( 'NONE',  ( -7.036662486785782988, 47.34139391789577189, 78.30609472687723382 ) ) ;
#1342 = ORIENTED_EDGE ( 'NONE', *, *, #19961, .T. ) ;
#1343 = CARTESIAN_POINT ( 'NONE',  ( 11.22215374030650281, 42.96218137147968008, 57.80715055817105252 ) ) ;
#1344 = CARTESIAN_POINT ( 'NONE',  ( -0.3452625352290130678, 52.31683812620389062, 75.52989945841051167 ) ) ;
#1345 = CARTESIAN_POINT ( 'NONE',  ( 0.5221537403065067418, 50.16218137147969713, 75.55433879953099563 ) ) ;
#1346 = CARTESIAN_POINT ( 'NONE',  ( -8.080465354403331801, 46.01554175503538602, 79.45433879953087342 ) ) ;
#1347 = EDGE_LOOP ( 'NONE', ( #6464, #10404, #6947, #17473 ) ) ;
#1348 = VECTOR ( 'NONE', #3895, 1000.000000000000114 ) ;
#1349 = LINE ( 'NONE', #3045, #6807 ) ;
#1350 = ORIENTED_EDGE ( 'NONE', *, *, #15478, .F. ) ;
#1351 = CARTESIAN_POINT ( 'NONE',  ( -3.934466035114216442, 36.51369227099507242, 75.53057231289058393 ) ) ;
#1352 = CARTESIAN_POINT ( 'NONE',  ( -4.256347323304533248, 37.50608895441494894, 75.99117330331094422 ) ) ;
#1353 = DIRECTION ( 'NONE',  ( 1.779391786395883536E-16, 5.922860397471806844E-17, -1.000000000000000000 ) ) ;
#1354 = ORIENTED_EDGE ( 'NONE', *, *, #15753, .T. ) ;
#1355 = CARTESIAN_POINT ( 'NONE',  ( 4.579592178280777581, 52.10552964593085790, 78.58658920843723195 ) ) ;
#1356 = FACE_OUTER_BOUND ( 'NONE', #10590, .T. ) ;
#1357 = CARTESIAN_POINT ( 'NONE',  ( 5.053692675489761754, 42.04909006277621586, 93.89183879953097289 ) ) ;
#1358 = VECTOR ( 'NONE', #6848, 1000.000000000000114 ) ;
#1359 = VECTOR ( 'NONE', #409, 1000.000000000000000 ) ;
#1360 = ORIENTED_EDGE ( 'NONE', *, *, #20955, .F. ) ;
#1361 = CARTESIAN_POINT ( 'NONE',  ( 8.443422548343662015, 42.04239353520513589, 78.13669174070733447 ) ) ;
#1362 = CARTESIAN_POINT ( 'NONE',  ( 11.22215374030649926, 42.76218137147968434, 80.55433879953099563 ) ) ;
#1363 = PLANE ( 'NONE',  #17340 ) ;
#1364 = CARTESIAN_POINT ( 'NONE',  ( 5.611423337425062385, 41.22389019960463230, 90.33621380123798872 ) ) ;
#1365 = CARTESIAN_POINT ( 'NONE',  ( 5.025485839985549319, 41.56218137147963887, 89.78933880294498238 ) ) ;
#1366 = AXIS2_PLACEMENT_3D ( 'NONE', #7617, #14410, #12614 ) ;
#1367 = VECTOR ( 'NONE', #14316, 1000.000000000000000 ) ;
#1368 = CARTESIAN_POINT ( 'NONE',  ( -7.496435415918218048, 40.53612117468122733, 79.30582264914816903 ) ) ;
#1369 = CARTESIAN_POINT ( 'NONE',  ( 0.6326014232273523552, 51.36153429190470376, 79.54845644658969661 ) ) ;
#1370 = CARTESIAN_POINT ( 'NONE',  ( -0.6022041793465181536, 52.97723187893011954, 79.21387586705148465 ) ) ;
#1371 = AXIS2_PLACEMENT_3D ( 'NONE', #13854, #12279, #18326 ) ;
#1372 = VERTEX_POINT ( 'NONE', #695 ) ;
#1373 = CARTESIAN_POINT ( 'NONE',  ( -4.314207556397965604, 37.54021473506075068, 75.97461220940198245 ) ) ;
#1374 = DIRECTION ( 'NONE',  ( -1.000000000000000000, -1.402518428993809243E-16, 6.308085367188358095E-15 ) ) ;
#1375 = CARTESIAN_POINT ( 'NONE',  ( 0.5706356501935867520, 52.36203804732553380, 75.97198585835440099 ) ) ;
#1376 = ORIENTED_EDGE ( 'NONE', *, *, #9773, .F. ) ;
#1377 = VERTEX_POINT ( 'NONE', #13991 ) ;
#1378 = CARTESIAN_POINT ( 'NONE',  ( 2.522153740306505298, 50.16218137147969713, 85.55433879953100984 ) ) ;
#1379 = CARTESIAN_POINT ( 'NONE',  ( -4.879976564110344306, 37.21210281127716968, 78.77850703318271997 ) ) ;
#1380 = LINE ( 'NONE', #20835, #8973 ) ;
#1381 = B_SPLINE_SURFACE_WITH_KNOTS ( 'NONE', 3, 1, ( 
 ( #17108, #14117 ),
 ( #10847, #12526 ),
 ( #19121, #12327 ),
 ( #2632, #8923 ),
 ( #17315, #18807 ),
 ( #14016, #20499 ),
 ( #5931, #6136 ),
 ( #19013, #16997 ),
 ( #12214, #2532 ),
 ( #2845, #15411 ),
 ( #9027, #15514 ),
 ( #4219, #12428 ),
 ( #17419, #7528 ),
 ( #1245, #9348 ),
 ( #2740, #1149 ),
 ( #7738, #12639 ),
 ( #1355, #71 ),
 ( #16146, #4533 ),
 ( #17619, #3163 ) ),
 .UNSPECIFIED., .F., .F., .F.,
 ( 4, 1, 1, 1, 1, 1, 1, 1, 1, 1, 1, 1, 1, 1, 1, 1, 4 ),
 ( 2, 2 ),
 ( 0.000000000000000000, 0.09548257688036490554, 0.1831260162920692325, 0.2638843215906733763, 0.3377405854367836469, 0.4051287172156797234, 0.4664893278449969150, 0.5228337310946251648, 0.5750047063118850499, 0.6251976803793458659, 0.6747285784134858799, 0.7246222549260739054, 0.7756163566473811555, 0.8279184090424840381, 0.8823814665238148836, 0.9394578349448057253, 1.000000000000000000 ),
 ( 0.000000000000000000, 1.000000000000000000 ),
 .UNSPECIFIED. ) ;
#1382 = CARTESIAN_POINT ( 'NONE',  ( 11.22215374030650281, 42.96218137147968008, 65.80574467885102763 ) ) ;
#1383 = VECTOR ( 'NONE', #14886, 1000.000000000000114 ) ;
#1384 = CARTESIAN_POINT ( 'NONE',  ( 8.623636628666181636, 43.00372860211926707, 77.60952670463396430 ) ) ;
#1385 = FACE_OUTER_BOUND ( 'NONE', #20347, .T. ) ;
#1386 = LINE ( 'NONE', #11291, #19153 ) ;
#1387 = VERTEX_POINT ( 'NONE', #2510 ) ;
#1388 = CARTESIAN_POINT ( 'NONE',  ( 33.03948732994508930, 43.16218137147969003, 78.80433879953099563 ) ) ;
#1389 = B_SPLINE_CURVE_WITH_KNOTS ( 'NONE', 3,
 ( #3693, #19863, #2317, #829, #8502, #12114, #6890, #2115 ),
 .UNSPECIFIED., .F., .F.,
 ( 4, 2, 2, 4 ),
 ( 0.000000000000000000, 0.0002990918838428522860, 0.0004486378257642822508, 0.0005981837676857122699 ),
 .UNSPECIFIED. ) ;
#1390 = DIRECTION ( 'NONE',  ( 1.000000000000000000, 1.402518428993831183E-16, -4.865963288531424442E-32 ) ) ;
#1391 = ADVANCED_FACE ( 'NONE', ( #7503 ), #13879, .F. ) ;
#1392 = CARTESIAN_POINT ( 'NONE',  ( 2.029186242314200861, 35.35002428291939225, 76.86610350541323555 ) ) ;
#1393 = ORIENTED_EDGE ( 'NONE', *, *, #520, .T. ) ;
#1394 = DIRECTION ( 'NONE',  ( 1.193617070626243484E-16, 1.000000000000000000, 0.000000000000000000 ) ) ;
#1395 = CARTESIAN_POINT ( 'NONE',  ( -5.058133621542618030, 44.89684013992257405, 91.74246380294499659 ) ) ;
#1396 = VERTEX_POINT ( 'NONE', #18460 ) ;
#1397 = CARTESIAN_POINT ( 'NONE',  ( -1.077846259693493458, 49.76218137147969856, 61.55433879953100273 ) ) ;
#1398 = CARTESIAN_POINT ( 'NONE',  ( 8.324322233486002531, 41.69710151208300175, 78.09303657357962436 ) ) ;
#1399 = DIRECTION ( 'NONE',  ( -1.402518428993831183E-16, 1.000000000000000000, -3.469446951953617640E-16 ) ) ;
#1400 = LINE ( 'NONE', #19165, #81 ) ;
#1401 = ORIENTED_EDGE ( 'NONE', *, *, #11885, .F. ) ;
#1402 = AXIS2_PLACEMENT_3D ( 'NONE', #17657, #12367, #18843 ) ;
#1403 =( BOUNDED_CURVE ( )  B_SPLINE_CURVE ( 3, ( #735, #6999, #842, #517 ),
 .UNSPECIFIED., .F., .F. ) 
 B_SPLINE_CURVE_WITH_KNOTS ( ( 4, 4 ),
 ( 2.801755744135677073, 3.481429563043919373 ),
 .UNSPECIFIED. ) 
 CURVE ( )  GEOMETRIC_REPRESENTATION_ITEM ( )  RATIONAL_B_SPLINE_CURVE ( ( 1.000000000000000000, 0.9618726943880423486, 0.9618726943880423486, 1.000000000000000000 ) ) 
 REPRESENTATION_ITEM ( '' )  );
#1404 = LINE ( 'NONE', #7587, #4734 ) ;
#1405 = EDGE_CURVE ( 'NONE', #15226, #4372, #4197, .T. ) ;
#1406 = ORIENTED_EDGE ( 'NONE', *, *, #4152, .F. ) ;
#1407 = DIRECTION ( 'NONE',  ( -4.818676322157797375E-16, -1.000000000000000000, 0.000000000000000000 ) ) ;
#1408 = B_SPLINE_CURVE_WITH_KNOTS ( 'NONE', 3,
 ( #6514, #16210, #8547, #20969, #18120, #11534, #136, #1635, #6404, #6615, #12911, #19392, #4808, #3637, #3226, #5016, #4909, #11329, #1851 ),
 .UNSPECIFIED., .F., .F.,
 ( 4, 1, 1, 1, 1, 1, 1, 1, 1, 1, 1, 1, 1, 1, 1, 1, 4 ),
 ( 0.000000000000000000, 0.07046818618994758754, 0.1352139183126853383, 0.1951004221781245107, 0.2505542266086520642, 0.3026661728221104464, 0.3524186183690131702, 0.4011907228821319227, 0.4500572973727005044, 0.5012199576353847386, 0.5567639849620312775, 0.6168130928284528691, 0.6819767269214894734, 0.7529340711039560485, 0.8292206168931396393, 0.9117786016023526896, 1.000000000000000000 ),
 .UNSPECIFIED. ) ;
#1409 = CARTESIAN_POINT ( 'NONE',  ( 28.52215374030649997, 44.16218137147968292, 93.55433879953098142 ) ) ;
#1410 = CARTESIAN_POINT ( 'NONE',  ( -7.480639693313347216, 47.82437745672348228, 78.83519423975563711 ) ) ;
#1411 = CARTESIAN_POINT ( 'NONE',  ( -1.477846259693495146, 50.16218137147969713, 82.55433879953099563 ) ) ;
#1412 = CARTESIAN_POINT ( 'NONE',  ( -5.943920255163962274, 37.99799515759236357, 76.35020017089209432 ) ) ;
#1413 = EDGE_CURVE ( 'NONE', #17717, #18484, #8482, .T. ) ;
#1414 = AXIS2_PLACEMENT_3D ( 'NONE', #9438, #15825, #11140 ) ;
#1415 = ORIENTED_EDGE ( 'NONE', *, *, #10439, .F. ) ;
#1416 = FACE_OUTER_BOUND ( 'NONE', #13377, .T. ) ;
#1417 = VECTOR ( 'NONE', #14612, 1000.000000000000114 ) ;
#1418 = EDGE_CURVE ( 'NONE', #5621, #11839, #2399, .T. ) ;
#1419 = EDGE_CURVE ( 'NONE', #19018, #15529, #2286, .T. ) ;
#1420 = ORIENTED_EDGE ( 'NONE', *, *, #13310, .F. ) ;
#1421 = DIRECTION ( 'NONE',  ( 1.110223024625156540E-16, 1.000000000000000000, 5.922860397471808077E-17 ) ) ;
#1422 = CARTESIAN_POINT ( 'NONE',  ( 3.460444912181559474, 49.25145096859824889, 95.64871380123798872 ) ) ;
#1423 = CARTESIAN_POINT ( 'NONE',  ( -1.677846259693499542, 44.16218137147969003, 37.95170767603170248 ) ) ;
#1424 = EDGE_LOOP ( 'NONE', ( #5177, #9020, #16881, #15243 ) ) ;
#1425 = DIRECTION ( 'NONE',  ( -0.9534635866061451637, -0.3015081906286224411, -2.009271279954815058E-16 ) ) ;
#1426 = CARTESIAN_POINT ( 'NONE',  ( 11.22215374030649926, 42.76218137147968434, 80.55433879953099563 ) ) ;
#1427 = CARTESIAN_POINT ( 'NONE',  ( 4.556677822976353376, 36.22933235006951946, 75.83703142516586126 ) ) ;
#1428 = DIRECTION ( 'NONE',  ( 1.193617070626243237E-16, 1.000000000000000000, 1.876284981264363171E-30 ) ) ;
#1429 = EDGE_CURVE ( 'NONE', #983, #18875, #11987, .T. ) ;
#1430 = CARTESIAN_POINT ( 'NONE',  ( 5.074809179647884250, 37.34648547976750166, 77.45531005930804724 ) ) ;
#1431 = ORIENTED_EDGE ( 'NONE', *, *, #12448, .F. ) ;
#1432 = CARTESIAN_POINT ( 'NONE',  ( -3.857944742499960888, 47.10944688436405414, 92.55433879953096721 ) ) ;
#1433 = DIRECTION ( 'NONE',  ( -0.9534635866061451637, -0.3015081906286224411, -2.009271279954815058E-16 ) ) ;
#1434 = AXIS2_PLACEMENT_3D ( 'NONE', #5372, #13689, #8597 ) ;
#1435 = EDGE_LOOP ( 'NONE', ( #18300, #20002 ) ) ;
#1436 = CARTESIAN_POINT ( 'NONE',  ( 1.953869608722836881, 49.18494452436591757, 95.05433879953099563 ) ) ;
#1437 = DIRECTION ( 'NONE',  ( -0.9534635866061452747, -0.3015081906286225522, -2.009271279954815797E-16 ) ) ;
#1438 = VECTOR ( 'NONE', #17781, 1000.000000000000114 ) ;
#1439 = FACE_OUTER_BOUND ( 'NONE', #700, .T. ) ;
#1440 = CARTESIAN_POINT ( 'NONE',  ( 0.7582201636353292917, 49.56899138526064519, 91.46996379611699979 ) ) ;
#1441 = FACE_OUTER_BOUND ( 'NONE', #11776, .T. ) ;
#1442 = CYLINDRICAL_SURFACE ( 'NONE', #4857, 4.000000000000000000 ) ;
#1443 = CARTESIAN_POINT ( 'NONE',  ( -3.053385034718948177, 36.78770617509731267, 76.68008248600652621 ) ) ;
#1444 = ORIENTED_EDGE ( 'NONE', *, *, #9410, .F. ) ;
#1445 = CARTESIAN_POINT ( 'NONE',  ( 2.050960264585806936, 52.82843088445552837, 77.27574491810834445 ) ) ;
#1446 = CARTESIAN_POINT ( 'NONE',  ( -3.539401246598059991, 43.09270903039240608, 79.40903933791013003 ) ) ;
#1447 = ADVANCED_FACE ( 'NONE', ( #9106 ), #20249, .F. ) ;
#1448 = ORIENTED_EDGE ( 'NONE', *, *, #12563, .F. ) ;
#1449 = VECTOR ( 'NONE', #2857, 1000.000000000000114 ) ;
#1450 = CARTESIAN_POINT ( 'NONE',  ( 5.928963754087451576, 43.92611494815086814, 92.71996379953098710 ) ) ;
#1451 = EDGE_CURVE ( 'NONE', #12015, #6821, #5227, .T. ) ;
#1452 = DIRECTION ( 'NONE',  ( -0.7071067811865434649, -0.7071067811865515695, 0.000000000000000000 ) ) ;
#1453 = CARTESIAN_POINT ( 'NONE',  ( 9.201390675156970289, 42.37087608097247227, 79.34093170394821470 ) ) ;
#1454 = CIRCLE ( 'NONE', #13345, 8.199999999999995737 ) ;
#1455 = DIRECTION ( 'NONE',  ( -1.239088197126290817E-16, -1.000000000000000000, 0.000000000000000000 ) ) ;
#1456 = ORIENTED_EDGE ( 'NONE', *, *, #7029, .T. ) ;
#1457 = CARTESIAN_POINT ( 'NONE',  ( 5.627315617218822119, 51.33161854646183997, 78.02054163389647101 ) ) ;
#1458 = ORIENTED_EDGE ( 'NONE', *, *, #3170, .T. ) ;
#1459 = CARTESIAN_POINT ( 'NONE',  ( -3.674734132037355661, 36.32183877683144857, 75.77010869825431882 ) ) ;
#1460 = CARTESIAN_POINT ( 'NONE',  ( 8.296628936784257391, 41.55497301399228149, 78.93669174070734584 ) ) ;
#1461 = EDGE_CURVE ( 'NONE', #264, #4065, #10399, .T. ) ;
#1462 = CARTESIAN_POINT ( 'NONE',  ( 4.393996117251955269, 36.11308595931626542, 76.73963291717792856 ) ) ;
#1463 = ORIENTED_EDGE ( 'NONE', *, *, #14279, .T. ) ;
#1464 = CARTESIAN_POINT ( 'NONE',  ( -4.436679849166036860, 37.65941850380397682, 77.31392376534303423 ) ) ;
#1465 = FACE_OUTER_BOUND ( 'NONE', #443, .T. ) ;
#1466 = CARTESIAN_POINT ( 'NONE',  ( 5.220616844236031007, 45.87228208810806507, 92.79808879953097289 ) ) ;
#1467 = EDGE_CURVE ( 'NONE', #4298, #3641, #18885, .T. ) ;
#1468 = VERTEX_POINT ( 'NONE', #4293 ) ;
#1469 = DIRECTION ( 'NONE',  ( 1.540237394707284220E-16, 1.793354297423764243E-16, -1.000000000000000000 ) ) ;
#1470 = LINE ( 'NONE', #1675, #17236 ) ;
#1471 = DIRECTION ( 'NONE',  ( 3.893792155548169402E-16, 7.183611964723547524E-17, -1.000000000000000000 ) ) ;
#1472 = CARTESIAN_POINT ( 'NONE',  ( -3.350035803220276609, 49.20851703305431357, 93.38308880123798872 ) ) ;
#1473 = AXIS2_PLACEMENT_3D ( 'NONE', #739, #6909, #5527 ) ;
#1474 = DIRECTION ( 'NONE',  ( 1.110223024625156540E-16, 1.000000000000000000, 5.922860397471808077E-17 ) ) ;
#1475 = DIRECTION ( 'NONE',  ( -0.9534635866061451637, -0.3015081906286224411, -2.009271279954815058E-16 ) ) ;
#1476 = CARTESIAN_POINT ( 'NONE',  ( -7.774959294756113692, 41.22996117453095621, 78.61536821129558916 ) ) ;
#1477 = CARTESIAN_POINT ( 'NONE',  ( -0.9388773962491546721, 52.84004908296358138, 77.21536821129558348 ) ) ;
#1478 = CARTESIAN_POINT ( 'NONE',  ( -0.7827652907628513956, 52.97865566965094786, 79.01146473771775902 ) ) ;
#1479 = VERTEX_POINT ( 'NONE', #8685 ) ;
#1480 = FACE_OUTER_BOUND ( 'NONE', #2363, .T. ) ;
#1481 = CARTESIAN_POINT ( 'NONE',  ( 0.5221537403065015237, 44.16218137147968292, 75.45433879953088763 ) ) ;
#1482 = CARTESIAN_POINT ( 'NONE',  ( 0.6277305834145071595, 52.36170047174137210, 75.97329779118079784 ) ) ;
#1483 = FACE_OUTER_BOUND ( 'NONE', #4375, .T. ) ;
#1484 = ORIENTED_EDGE ( 'NONE', *, *, #18701, .T. ) ;
#1485 = CIRCLE ( 'NONE', #20502, 3.999999999999996447 ) ;
#1486 = EDGE_CURVE ( 'NONE', #8055, #5056, #5581, .T. ) ;
#1487 = B_SPLINE_CURVE_WITH_KNOTS ( 'NONE', 3,
 ( #9600, #12991, #11192, #12880, #9704, #17874, #4777, #9916, #16498, #16183, #8410, #8198, #18093, #110, #19567, #17775, #16401, #14685, #13199, #3296, #6587, #7991, #1824, #19362, #3097, #17980, #16287, #17664, #1608, #19673, #6693 ),
 .UNSPECIFIED., .F., .F.,
 ( 4, 1, 1, 1, 1, 1, 1, 1, 1, 1, 1, 1, 1, 1, 1, 1, 1, 1, 1, 1, 1, 1, 1, 1, 1, 1, 1, 1, 4 ),
 ( 0.000000000000000000, 0.04402879139878041609, 0.08604540006880039005, 0.1260521755942069777, 0.1641511405281330660, 0.2003442918647115323, 0.2347805632357193584, 0.2676267374383518027, 0.2986515534027265328, 0.3283031585252670914, 0.3570062744687346745, 0.3846398569069188755, 0.4113091075058319390, 0.4372322170293685417, 0.4625237182236557887, 0.4872935253130181721, 0.5115235732650775802, 0.5580727247437320404, 0.6018864549903041317, 0.6437727082467282758, 0.6848253805047307408, 0.7076001045990409910, 0.7352252901417971609, 0.7674583008524621386, 0.8043075748156178761, 0.8460289209228792906, 0.8926357087385640154, 0.9438729761760307202, 1.000000000000000000 ),
 .UNSPECIFIED. ) ;
#1488 = LINE ( 'NONE', #18073, #11449 ) ;
#1489 = LINE ( 'NONE', #9580, #3300 ) ;
#1490 = CARTESIAN_POINT ( 'NONE',  ( 5.085125551764789087, 37.34896360483502775, 77.63600869567171969 ) ) ;
#1491 = CARTESIAN_POINT ( 'NONE',  ( -6.354755732003290802, 42.02918051195119631, 76.16022115247204738 ) ) ;
#1492 = CARTESIAN_POINT ( 'NONE',  ( 2.891178777371211428, 49.58011692477155208, 94.26356103946022813 ) ) ;
#1493 = CARTESIAN_POINT ( 'NONE',  ( 6.284457548606577681, 49.99629437706096979, 77.78632772248469962 ) ) ;
#1494 = CARTESIAN_POINT ( 'NONE',  ( -4.792503378000012582, 37.91763016944491227, 72.45433879953085921 ) ) ;
#1495 = CARTESIAN_POINT ( 'NONE',  ( 9.353187571392870936, 42.82582100880699016, 77.22643688620827618 ) ) ;
#1496 = DIRECTION ( 'NONE',  ( 0.9534635866061470511, 0.3015081906286169455, 2.009271279954808648E-16 ) ) ;
#1497 = CARTESIAN_POINT ( 'NONE',  ( 6.961907239250668233, 50.34580947589670075, 76.63889762306028786 ) ) ;
#1498 = VECTOR ( 'NONE', #8770, 1000.000000000000000 ) ;
#1499 = DIRECTION ( 'NONE',  ( -1.402518428993830937E-16, 1.000000000000000000, -3.469446951953617147E-16 ) ) ;
#1500 = ADVANCED_FACE ( 'NONE', ( #902 ), #15166, .T. ) ;
#1501 = CARTESIAN_POINT ( 'NONE',  ( -4.740836738068939127, 51.21721328354402658, 79.54427050475041483 ) ) ;
#1502 = CARTESIAN_POINT ( 'NONE',  ( 5.244278063348997598, 50.86602667680485723, 78.70784175427819207 ) ) ;
#1503 = EDGE_LOOP ( 'NONE', ( #15950, #6051, #18646, #9291 ) ) ;
#1504 = CARTESIAN_POINT ( 'NONE',  ( 0.5221537403065015237, 44.16218137147968292, 75.45433879953088763 ) ) ;
#1505 = CARTESIAN_POINT ( 'NONE',  ( 28.09439724277525130, 40.36218137147969287, 87.65433879953101837 ) ) ;
#1506 = ORIENTED_EDGE ( 'NONE', *, *, #13097, .T. ) ;
#1507 = CARTESIAN_POINT ( 'NONE',  ( 5.397982717164803823, 37.75027360759684569, 75.36337631951366234 ) ) ;
#1508 = CARTESIAN_POINT ( 'NONE',  ( 5.086801335794131518, 51.73087467290688579, 79.44143248960128290 ) ) ;
#1509 = DIRECTION ( 'NONE',  ( -1.301042606982606060E-16, -1.000000000000000000, 0.000000000000000000 ) ) ;
#1510 = CARTESIAN_POINT ( 'NONE',  ( 0.8383241538550171290, 52.35221990523898938, 76.16511824318942558 ) ) ;
#1511 = LINE ( 'NONE', #17881, #7558 ) ;
#1512 = ORIENTED_EDGE ( 'NONE', *, *, #9923, .T. ) ;
#1513 = CARTESIAN_POINT ( 'NONE',  ( 5.847824973458005005, 37.15193883188941015, 77.47236191065434241 ) ) ;
#1514 = ORIENTED_EDGE ( 'NONE', *, *, #5438, .F. ) ;
#1515 = CARTESIAN_POINT ( 'NONE',  ( -4.524181921268124462, 40.28999182795290324, 96.03933880123798872 ) ) ;
#1516 = ADVANCED_FACE ( 'NONE', ( #18566, #20149 ), #3978, .T. ) ;
#1517 = CARTESIAN_POINT ( 'NONE',  ( -4.567115856812060670, 47.10047254335474065, 92.05496380123798872 ) ) ;
#1518 = CARTESIAN_POINT ( 'NONE',  ( -0.001084937681666381338, 35.97658959305408644, 77.43518796918013436 ) ) ;
#1519 = DIRECTION ( 'NONE',  ( -1.402518428993830937E-16, 1.000000000000000000, -3.469446951953617147E-16 ) ) ;
#1520 = CARTESIAN_POINT ( 'NONE',  ( -7.940942381894581459, 41.72644817493324609, 78.82529883526802905 ) ) ;
#1521 = ORIENTED_EDGE ( 'NONE', *, *, #6169, .F. ) ;
#1522 = CARTESIAN_POINT ( 'NONE',  ( 8.214799251806553571, 41.32260305165857517, 76.40801527011910821 ) ) ;
#1523 = ADVANCED_FACE ( 'NONE', ( #14189 ), #9551, .T. ) ;
#1524 = ORIENTED_EDGE ( 'NONE', *, *, #12510, .T. ) ;
#1525 = CARTESIAN_POINT ( 'NONE',  ( -5.838428831739583380, 50.43291415881836315, 78.10580938776615767 ) ) ;
#1526 = EDGE_CURVE ( 'NONE', #2157, #1583, #5812, .T. ) ;
#1527 = CARTESIAN_POINT ( 'NONE',  ( 1.119863296874942682, 50.25084051303457500, 77.06567965797613340 ) ) ;
#1528 = CARTESIAN_POINT ( 'NONE',  ( -7.098692764276762546, 41.50643870456164564, 78.36017682096837689 ) ) ;
#1529 = ORIENTED_EDGE ( 'NONE', *, *, #17457, .F. ) ;
#1530 = CARTESIAN_POINT ( 'NONE',  ( 8.527988662190095326, 48.03182059810101379, 79.44551527011911674 ) ) ;
#1531 = CARTESIAN_POINT ( 'NONE',  ( -4.901157372041539340, 42.48549306292126460, 95.05433879953096721 ) ) ;
#1532 = CARTESIAN_POINT ( 'NONE',  ( 5.956414982595287455, 44.61570594562444114, 92.55433879953099563 ) ) ;
#1533 = CARTESIAN_POINT ( 'NONE',  ( 5.215133383782184495, 50.88144501658546659, 76.13411024644928204 ) ) ;
#1534 = CARTESIAN_POINT ( 'NONE',  ( 5.467161035934759994, 36.87993031913157438, 77.68578589458712713 ) ) ;
#1535 = ORIENTED_EDGE ( 'NONE', *, *, #12438, .T. ) ;
#1536 = DIRECTION ( 'NONE',  ( 0.9534635866061452747, 0.3015081906286224966, 2.009271279954815304E-16 ) ) ;
#1537 = CARTESIAN_POINT ( 'NONE',  ( 1.011011570371347812, 52.34791438083374260, 76.77344599742670539 ) ) ;
#1538 = ORIENTED_EDGE ( 'NONE', *, *, #1461, .F. ) ;
#1539 = CARTESIAN_POINT ( 'NONE',  ( 4.101515559893016416, 47.72501102306959808, 95.05433879953095300 ) ) ;
#1540 = FACE_OUTER_BOUND ( 'NONE', #7776, .T. ) ;
#1541 = LINE ( 'NONE', #16121, #19270 ) ;
#1542 = CARTESIAN_POINT ( 'NONE',  ( 5.848951923618479931, 37.15274410921379911, 77.37492703482499223 ) ) ;
#1543 = CARTESIAN_POINT ( 'NONE',  ( 2.921181103050040306, 49.30691215337508737, 91.00121379782397923 ) ) ;
#1544 = FACE_OUTER_BOUND ( 'NONE', #5148, .T. ) ;
#1545 = B_SPLINE_CURVE_WITH_KNOTS ( 'NONE', 3,
 ( #1702, #19243, #19342, #4558, #14461, #1490, #16169, #12665, #94, #9373 ),
 .UNSPECIFIED., .F., .F.,
 ( 4, 2, 2, 2, 4 ),
 ( 0.000000000000000000, 0.0001199900948641854036, 0.0002399801897283708072, 0.0003599702845925562109, 0.0004799603794567416145 ),
 .UNSPECIFIED. ) ;
#1546 = LINE ( 'NONE', #8030, #12564 ) ;
#1547 = CARTESIAN_POINT ( 'NONE',  ( -3.165502623679720795, 36.87052292169065737, 77.44024473021482891 ) ) ;
#1548 = B_SPLINE_CURVE_WITH_KNOTS ( 'NONE', 3,
 ( #4535, #17523, #19014, #9349, #3052, #16249, #17835, #7637, #14540, #15835, #11262, #1567, #20697, #14118, #14433, #17733 ),
 .UNSPECIFIED., .F., .F.,
 ( 4, 2, 2, 2, 2, 2, 2, 4 ),
 ( 0.000000000000000000, 0.0001316607980626216534, 0.0002633215961252433068, 0.0005266431922504869389, 0.0007899647883757306794, 0.001053286384500974312, 0.001579929576751444662, 0.002106572769001915230 ),
 .UNSPECIFIED. ) ;
#1549 = VERTEX_POINT ( 'NONE', #20575 ) ;
#1550 = CARTESIAN_POINT ( 'NONE',  ( -7.132598987128367263, 47.10241527675634643, 78.19896882776124869 ) ) ;
#1551 = CARTESIAN_POINT ( 'NONE',  ( -3.955205046931959068, 36.52901134360648427, 77.68963291717793140 ) ) ;
#1552 = EDGE_LOOP ( 'NONE', ( #11027, #2531, #7948, #10259 ) ) ;
#1553 = DIRECTION ( 'NONE',  ( -0.9429220365244147528, 0.3330135628418914862, -8.551124769255465366E-17 ) ) ;
#1554 = EDGE_CURVE ( 'NONE', #14425, #6065, #15702, .T. ) ;
#1555 = CARTESIAN_POINT ( 'NONE',  ( -0.6451721385307191969, 52.27904522445349045, 75.73030909034207525 ) ) ;
#1556 = CARTESIAN_POINT ( 'NONE',  ( -2.077846259693550746, 39.65884927180063357, 96.66433879953098085 ) ) ;
#1557 = B_SPLINE_SURFACE_WITH_KNOTS ( 'NONE', 3, 1, ( 
 ( #9147, #14033 ),
 ( #10861, #15747 ),
 ( #12541, #19030 ),
 ( #15527, #13714 ),
 ( #18919, #16904 ),
 ( #839, #2757 ),
 ( #20514, #20189 ),
 ( #15639, #4018 ),
 ( #9260, #5619 ),
 ( #7325, #4335 ),
 ( #1164, #18606 ),
 ( #12229, #7650 ),
 ( #9041, #14129 ),
 ( #10541, #17012 ),
 ( #13814, #943 ),
 ( #7431, #20292 ),
 ( #4126, #10655 ),
 ( #17120, #2544 ),
 ( #13925, #20407 ) ),
 .UNSPECIFIED., .F., .F., .F.,
 ( 4, 1, 1, 1, 1, 1, 1, 1, 1, 1, 1, 1, 1, 1, 1, 1, 4 ),
 ( 2, 2 ),
 ( 0.000000000000000000, 0.09472651553281030701, 0.1809448578637775085, 0.2575849355004761199, 0.3257111939256314703, 0.3842597268839244573, 0.4332657528852557616, 0.4727039292014991179, 0.5037345896081361074, 0.5551104982754543338, 0.6060435029138766527, 0.6590687186606726256, 0.7172582036121251114, 0.7797016678215834551, 0.8463570695623257034, 0.9189979831805518140, 1.000000000000000000 ),
 ( 0.000000000000000000, 1.000000000000000000 ),
 .UNSPECIFIED. ) ;
#1558 = CARTESIAN_POINT ( 'NONE',  ( -3.012672749018421747, 51.56125195451731003, 76.00197347997514896 ) ) ;
#1559 = ORIENTED_EDGE ( 'NONE', *, *, #5348, .T. ) ;
#1560 = CARTESIAN_POINT ( 'NONE',  ( 5.599231707071657738, 51.35236299959863970, 78.30875056423674607 ) ) ;
#1561 = ORIENTED_EDGE ( 'NONE', *, *, #13796, .T. ) ;
#1562 = CARTESIAN_POINT ( 'NONE',  ( 2.722153740306517911, 44.16218137147969003, 56.15433879953099705 ) ) ;
#1563 = CARTESIAN_POINT ( 'NONE',  ( -4.158450310422142415, 37.43377637453095730, 76.36459416792565946 ) ) ;
#1564 = CARTESIAN_POINT ( 'NONE',  ( -0.2125050281363792815, 38.58189400963055959, 92.99246379953098085 ) ) ;
#1565 = ORIENTED_EDGE ( 'NONE', *, *, #18553, .F. ) ;
#1566 = CARTESIAN_POINT ( 'NONE',  ( -5.135517778528634558, 37.40086081253993910, 77.33633635728615729 ) ) ;
#1567 = CARTESIAN_POINT ( 'NONE',  ( -7.016336539762185076, 40.93177535399939160, 79.42775612813471753 ) ) ;
#1568 = CARTESIAN_POINT ( 'NONE',  ( 5.666884522201896424, 41.76315400873614436, 91.78246379782397923 ) ) ;
#1569 = ORIENTED_EDGE ( 'NONE', *, *, #4396, .T. ) ;
#1570 = LINE ( 'NONE', #5057, #7701 ) ;
#1571 = DIRECTION ( 'NONE',  ( 0.000000000000000000, 0.000000000000000000, 1.000000000000000000 ) ) ;
#1572 = CARTESIAN_POINT ( 'NONE',  ( -5.260605497331073188, 38.34791887000096722, 79.35384852091290497 ) ) ;
#1573 = ADVANCED_FACE ( 'NONE', ( #11332 ), #20893, .T. ) ;
#1574 =( NAMED_UNIT ( * ) SI_UNIT ( $, .STERADIAN. ) SOLID_ANGLE_UNIT ( ) );
#1575 = CARTESIAN_POINT ( 'NONE',  ( 3.460444912181559474, 49.25145096859824889, 92.99246380123798872 ) ) ;
#1576 = EDGE_CURVE ( 'NONE', #5980, #14474, #15264, .T. ) ;
#1577 = CARTESIAN_POINT ( 'NONE',  ( 5.885001432003880595, 37.95852707458993081, 78.35303564028859569 ) ) ;
#1578 = FACE_OUTER_BOUND ( 'NONE', #13552, .T. ) ;
#1579 = EDGE_CURVE ( 'NONE', #2109, #17272, #1672, .T. ) ;
#1580 = CARTESIAN_POINT ( 'NONE',  ( 5.632375035844972899, 36.99798619459680538, 75.36061873398452349 ) ) ;
#1581 = EDGE_CURVE ( 'NONE', #3682, #18429, #16956, .T. ) ;
#1582 = DIRECTION ( 'NONE',  ( -1.196361017915039239E-16, 0.000000000000000000, 1.000000000000000000 ) ) ;
#1583 = VERTEX_POINT ( 'NONE', #16526 ) ;
#1584 = DIRECTION ( 'NONE',  ( 0.7071067811865479058, -3.662367542345315236E-17, -0.7071067811865472397 ) ) ;
#1585 = CARTESIAN_POINT ( 'NONE',  ( 8.638892188706073227, 43.04945048335348901, 76.30013550906805619 ) ) ;
#1586 = CARTESIAN_POINT ( 'NONE',  ( 5.566326199328858415, 51.37666897265353327, 76.21945306000542075 ) ) ;
#1587 = CARTESIAN_POINT ( 'NONE',  ( 6.487242172018640396, 49.78241043515765085, 78.48669174070734300 ) ) ;
#1588 = EDGE_CURVE ( 'NONE', #13986, #8211, #7083, .T. ) ;
#1589 = ORIENTED_EDGE ( 'NONE', *, *, #16507, .T. ) ;
#1590 = AXIS2_PLACEMENT_3D ( 'NONE', #92, #11283, #19552 ) ;
#1591 = ORIENTED_EDGE ( 'NONE', *, *, #5839, .T. ) ;
#1592 = CARTESIAN_POINT ( 'NONE',  ( 7.770520676892109790, 40.32783022416316498, 75.85744100972826232 ) ) ;
#1593 = CARTESIAN_POINT ( 'NONE',  ( 0.5221537403064983041, 37.76218137147968434, 95.05433879953096721 ) ) ;
#1594 = CARTESIAN_POINT ( 'NONE',  ( 4.144921371010943822, 51.51850920521359001, 78.55031972648716021 ) ) ;
#1595 = FACE_OUTER_BOUND ( 'NONE', #19586, .T. ) ;
#1596 = CARTESIAN_POINT ( 'NONE',  ( 3.460444912181559474, 49.25145096859824889, 94.24246380123807398 ) ) ;
#1597 = LINE ( 'NONE', #19072, #17222 ) ;
#1598 = CARTESIAN_POINT ( 'NONE',  ( 6.862151516847506016, 50.41949500963030317, 77.39285358288198324 ) ) ;
#1599 = CARTESIAN_POINT ( 'NONE',  ( 8.617838889373357958, 45.46597658821364263, 78.74919174070734584 ) ) ;
#1600 = VECTOR ( 'NONE', #16532, 1000.000000000000000 ) ;
#1601 = CARTESIAN_POINT ( 'NONE',  ( 5.611423337425062385, 41.22389019960463230, 92.67996380123798872 ) ) ;
#1602 = ORIENTED_EDGE ( 'NONE', *, *, #15630, .T. ) ;
#1603 = EDGE_CURVE ( 'NONE', #11193, #1479, #19597, .T. ) ;
#1604 = CARTESIAN_POINT ( 'NONE',  ( -4.981196848641174846, 38.22287665415147018, 79.46937556254052026 ) ) ;
#1605 = CARTESIAN_POINT ( 'NONE',  ( -5.802311964739910621, 50.45872194965342317, 78.71528818263502103 ) ) ;
#1606 = DIRECTION ( 'NONE',  ( 0.9999689119394086223, -0.007885122365275665235, 1.526048693634353392E-16 ) ) ;
#1607 = CARTESIAN_POINT ( 'NONE',  ( 8.789147962602239517, 47.20595287382010241, 75.43669174070734584 ) ) ;
#1608 = CARTESIAN_POINT ( 'NONE',  ( 8.385851074499695912, 39.92665216093506331, 76.98031643592585738 ) ) ;
#1609 = ORIENTED_EDGE ( 'NONE', *, *, #4634, .T. ) ;
#1610 = CARTESIAN_POINT ( 'NONE',  ( 0.006406757820996506793, 52.97120749765745273, 75.41772606587693417 ) ) ;
#1611 = VECTOR ( 'NONE', #20422, 1000.000000000000000 ) ;
#1612 = CARTESIAN_POINT ( 'NONE',  ( 0.3970485124631613627, 52.20691167326921800, 79.54130260543404063 ) ) ;
#1613 = CARTESIAN_POINT ( 'NONE',  ( 6.853565520360258567, 37.87060420419414442, 77.68698088877128782 ) ) ;
#1614 = DIRECTION ( 'NONE',  ( -0.000000000000000000, 0.000000000000000000, 1.000000000000000000 ) ) ;
#1615 = LINE ( 'NONE', #11309, #1438 ) ;
#1616 = ORIENTED_EDGE ( 'NONE', *, *, #16806, .T. ) ;
#1617 = CARTESIAN_POINT ( 'NONE',  ( 11.22215374030650281, 42.76218137147968434, 58.20715055817105110 ) ) ;
#1618 = ORIENTED_EDGE ( 'NONE', *, *, #14327, .T. ) ;
#1619 = CARTESIAN_POINT ( 'NONE',  ( 6.828503391016846891, 43.33193468930419101, 90.25808880123800293 ) ) ;
#1620 = VECTOR ( 'NONE', #2773, 1000.000000000000227 ) ;
#1621 = CARTESIAN_POINT ( 'NONE',  ( 0.5706356501935867520, 52.36203804732553380, 75.97198585835440099 ) ) ;
#1622 = DIRECTION ( 'NONE',  ( 1.000000000000000000, 0.000000000000000000, 0.000000000000000000 ) ) ;
#1623 = CARTESIAN_POINT ( 'NONE',  ( 6.531299583006453524, 48.82481648921748274, 72.45432679953087529 ) ) ;
#1624 = AXIS2_PLACEMENT_3D ( 'NONE', #664, #10587, #10264 ) ;
#1625 = CARTESIAN_POINT ( 'NONE',  ( 0.5221537403065181771, 44.16218137147969003, 56.15433879953099705 ) ) ;
#1626 = ORIENTED_EDGE ( 'NONE', *, *, #1842, .F. ) ;
#1627 = CARTESIAN_POINT ( 'NONE',  ( -4.616992131696500579, 37.01784680471219247, 75.99117330331094422 ) ) ;
#1628 = ORIENTED_EDGE ( 'NONE', *, *, #523, .T. ) ;
#1629 = CARTESIAN_POINT ( 'NONE',  ( -1.477846259693495590, 49.16218137147968292, 82.55433879953099563 ) ) ;
#1630 = DIRECTION ( 'NONE',  ( 1.000000000000000000, -1.110223024625156171E-16, -4.142850521348544074E-16 ) ) ;
#1631 = CARTESIAN_POINT ( 'NONE',  ( -4.524181921268124462, 40.28999182795290324, 96.03933880123798872 ) ) ;
#1632 = ORIENTED_EDGE ( 'NONE', *, *, #18972, .F. ) ;
#1633 = EDGE_CURVE ( 'NONE', #10210, #11635, #138, .T. ) ;
#1634 = CARTESIAN_POINT ( 'NONE',  ( 2.106992520703838689, 52.20762236682631396, 77.55786177449368779 ) ) ;
#1635 = CARTESIAN_POINT ( 'NONE',  ( -5.803682309770399783, 37.89440703645915676, 79.21211992218960063 ) ) ;
#1636 = CIRCLE ( 'NONE', #18628, 6.000000000000002665 ) ;
#1637 = CARTESIAN_POINT ( 'NONE',  ( 4.786818451252839779, 47.27669862923430344, 92.55433879953093879 ) ) ;
#1638 = CARTESIAN_POINT ( 'NONE',  ( -4.035675179171060556, 50.97418048369974031, 78.65149807507090429 ) ) ;
#1639 = CARTESIAN_POINT ( 'NONE',  ( 5.435172323252741577, 36.85707235623052469, 77.60331851759366373 ) ) ;
#1640 = VERTEX_POINT ( 'NONE', #11536 ) ;
#1641 = CARTESIAN_POINT ( 'NONE',  ( -4.030452273627614268, 50.97791258077830889, 76.38961819735682468 ) ) ;
#1642 = DIRECTION ( 'NONE',  ( -5.626130192357176673E-16, -1.831515347669941892E-30, 1.000000000000000000 ) ) ;
#1643 = ORIENTED_EDGE ( 'NONE', *, *, #634, .T. ) ;
#1644 = CARTESIAN_POINT ( 'NONE',  ( 3.113867759335670726, 48.58372638270478205, 95.05433879953093879 ) ) ;
#1645 = DIRECTION ( 'NONE',  ( 0.000000000000000000, 0.000000000000000000, 1.000000000000000000 ) ) ;
#1646 = CARTESIAN_POINT ( 'NONE',  ( -7.075244453723417593, 44.52209897503762193, 75.45433879953087342 ) ) ;
#1647 = CARTESIAN_POINT ( 'NONE',  ( 2.232254456934872344, 39.46371826755015633, 92.17308879611698558 ) ) ;
#1648 = CARTESIAN_POINT ( 'NONE',  ( -7.677846259693480668, 36.96218137147968008, 50.15433879953098995 ) ) ;
#1649 = CARTESIAN_POINT ( 'NONE',  ( 11.22215374030650281, 42.76218137147968434, 78.80433879953099563 ) ) ;
#1650 = CARTESIAN_POINT ( 'NONE',  ( 5.146043734657006041, 40.41782908280415398, 90.15009084312077903 ) ) ;
#1651 = AXIS2_PLACEMENT_3D ( 'NONE', #3553, #677, #20020 ) ;
#1652 = CARTESIAN_POINT ( 'NONE',  ( 5.568159709253909462, 50.62067869072730275, 76.16996516156804375 ) ) ;
#1653 = ORIENTED_EDGE ( 'NONE', *, *, #6778, .T. ) ;
#1654 = CARTESIAN_POINT ( 'NONE',  ( 1.641182446559612318, 52.20525483714327208, 79.33873778842219338 ) ) ;
#1655 = EDGE_LOOP ( 'NONE', ( #2425, #7689, #3789, #6402 ) ) ;
#1656 = CARTESIAN_POINT ( 'NONE',  ( -4.225462782839600528, 50.84799750334796187, 79.54845644658969661 ) ) ;
#1657 = EDGE_CURVE ( 'NONE', #18483, #13663, #4708, .T. ) ;
#1658 = DIRECTION ( 'NONE',  ( 1.134288711164059445E-16, 1.000000000000000000, 7.183611964723549989E-17 ) ) ;
#1659 = CARTESIAN_POINT ( 'NONE',  ( 2.115041367457930033, 52.20598078514408513, 76.48963291717792856 ) ) ;
#1660 = CARTESIAN_POINT ( 'NONE',  ( -7.515910409428084193, 42.82581192461235986, 76.44005692701139765 ) ) ;
#1661 = VERTEX_POINT ( 'NONE', #3639 ) ;
#1662 = DIRECTION ( 'NONE',  ( -0.8043570849667760481, 0.5941461771851693774, -1.733862608106482338E-17 ) ) ;
#1663 = LINE ( 'NONE', #8147, #11664 ) ;
#1664 = ORIENTED_EDGE ( 'NONE', *, *, #2095, .T. ) ;
#1665 = DIRECTION ( 'NONE',  ( 0.000000000000000000, 0.000000000000000000, -1.000000000000000000 ) ) ;
#1666 = CARTESIAN_POINT ( 'NONE',  ( 8.375284547952256631, 41.80244594815106751, 78.79373795524233515 ) ) ;
#1667 = CARTESIAN_POINT ( 'NONE',  ( -3.981178359372548492, 46.76218137147973408, 93.85183879953099506 ) ) ;
#1668 = ORIENTED_EDGE ( 'NONE', *, *, #16638, .T. ) ;
#1669 = CARTESIAN_POINT ( 'NONE',  ( -1.477846259693492925, 49.16218137147969003, 66.55433879953099563 ) ) ;
#1670 = LINE ( 'NONE', #2085, #11217 ) ;
#1671 = CARTESIAN_POINT ( 'NONE',  ( 2.635245049009968366, 48.69372030666295359, 94.20433879953097289 ) ) ;
#1672 = CIRCLE ( 'NONE', #21018, 4.200000000000003730 ) ;
#1673 = EDGE_LOOP ( 'NONE', ( #17517, #15759, #16528, #10336 ) ) ;
#1674 = CARTESIAN_POINT ( 'NONE',  ( -2.313335635445065375, 50.56218137147968861, 95.05433879953096721 ) ) ;
#1675 = CARTESIAN_POINT ( 'NONE',  ( -1.077846259693497677, 50.16218137147969713, 85.55433879953100984 ) ) ;
#1676 = PLANE ( 'NONE',  #11562 ) ;
#1677 = CARTESIAN_POINT ( 'NONE',  ( 5.568489401881125289, 48.03437091500646261, 94.16433880123797451 ) ) ;
#1678 =( LENGTH_UNIT ( ) NAMED_UNIT ( * ) SI_UNIT ( .MILLI., .METRE. ) );
#1679 = UNCERTAINTY_MEASURE_WITH_UNIT (LENGTH_MEASURE( 1.000000000000000082E-05 ), #18708, 'distance_accuracy_value', 'NONE');
#1680 = EDGE_CURVE ( 'NONE', #10288, #12015, #16432, .T. ) ;
#1681 = CARTESIAN_POINT ( 'NONE',  ( -5.838255805151811195, 50.43303779728307745, 76.65235776097600251 ) ) ;
#1682 = CARTESIAN_POINT ( 'NONE',  ( 0.4501203527806490468, 52.96713143748286257, 76.95466777776533718 ) ) ;
#1683 = CARTESIAN_POINT ( 'NONE',  ( -7.677846259693481556, 40.96218137147969429, 95.05433879953098142 ) ) ;
#1684 = VECTOR ( 'NONE', #4285, 1000.000000000000000 ) ;
#1685 = CARTESIAN_POINT ( 'NONE',  ( 7.870074787697994623, 40.74525595966579772, 79.37958223971880045 ) ) ;
#1686 = ORIENTED_EDGE ( 'NONE', *, *, #4099, .T. ) ;
#1687 = CARTESIAN_POINT ( 'NONE',  ( -4.477846259693498254, 37.66218137147969713, 53.35433879953099989 ) ) ;
#1688 = CARTESIAN_POINT ( 'NONE',  ( 0.5221537403065020788, 52.36218137147968577, 83.03825919817350609 ) ) ;
#1689 = EDGE_CURVE ( 'NONE', #13226, #14563, #13229, .T. ) ;
#1690 = LINE ( 'NONE', #14764, #8252 ) ;
#1691 = CARTESIAN_POINT ( 'NONE',  ( 6.924055141134583202, 50.37376929599953712, 78.48669174070734300 ) ) ;
#1692 = EDGE_CURVE ( 'NONE', #4602, #7376, #342, .T. ) ;
#1693 = EDGE_CURVE ( 'NONE', #10499, #8207, #11747, .T. ) ;
#1694 = ORIENTED_EDGE ( 'NONE', *, *, #11419, .F. ) ;
#1695 = CIRCLE ( 'NONE', #16298, 3.999999999999996447 ) ;
#1696 = CARTESIAN_POINT ( 'NONE',  ( 5.513895972565329373, 50.66228159254415431, 78.86250487280319987 ) ) ;
#1697 = ORIENTED_EDGE ( 'NONE', *, *, #19263, .F. ) ;
#1698 = AXIS2_PLACEMENT_3D ( 'NONE', #13134, #14414, #12927 ) ;
#1699 = CARTESIAN_POINT ( 'NONE',  ( -1.077846259693492348, 47.82824192744436687, 53.55433879953100273 ) ) ;
#1700 = DIRECTION ( 'NONE',  ( -1.000000000000000000, 1.110223024625156540E-16, -1.779391786395883043E-16 ) ) ;
#1701 = ADVANCED_FACE ( 'NONE', ( #8549 ), #452, .F. ) ;
#1702 = CARTESIAN_POINT ( 'NONE',  ( 5.282950423531485917, 37.48574407745871895, 77.76022115247205591 ) ) ;
#1703 = CARTESIAN_POINT ( 'NONE',  ( 2.463659247115866258, 38.82793883177424732, 94.12621379782399345 ) ) ;
#1704 = FACE_OUTER_BOUND ( 'NONE', #12263, .T. ) ;
#1705 = VECTOR ( 'NONE', #4961, 1000.000000000000227 ) ;
#1706 = CARTESIAN_POINT ( 'NONE',  ( 6.518026314581760516, 49.74885348734871116, 76.80946857459053945 ) ) ;
#1707 = CARTESIAN_POINT ( 'NONE',  ( 4.553522022787977797, 51.30320697278853004, 77.72474235116990826 ) ) ;
#1708 = CARTESIAN_POINT ( 'NONE',  ( -1.598719209087999138, 36.85794301744668644, 75.45433879953087342 ) ) ;
#1709 = AXIS2_PLACEMENT_3D ( 'NONE', #6936, #13441, #14615 ) ;
#1710 = CLOSED_SHELL ( 'NONE', ( #6618, #7033, #20532, #5509, #19337, #2964, #5868, #9510, #12390, #11712, #10881, #5277 ) ) ;
#1711 = ORIENTED_EDGE ( 'NONE', *, *, #6470, .T. ) ;
#1712 = CARTESIAN_POINT ( 'NONE',  ( -5.510796958474739604, 38.60848837797752964, 72.45433879953085921 ) ) ;
#1713 = CARTESIAN_POINT ( 'NONE',  ( 8.871704507997348443, 41.38278572309461367, 78.93627637315103129 ) ) ;
#1714 = DIRECTION ( 'NONE',  ( -1.000000000000000000, 0.000000000000000000, 0.000000000000000000 ) ) ;
#1715 = VECTOR ( 'NONE', #15071, 1000.000000000000000 ) ;
#1716 = VECTOR ( 'NONE', #16757, 1000.000000000000000 ) ;
#1717 = CARTESIAN_POINT ( 'NONE',  ( -4.477846259693478714, 37.66295064777091994, 54.55433879953098852 ) ) ;
#1718 = EDGE_CURVE ( 'NONE', #10129, #2084, #3229, .T. ) ;
#1719 = CARTESIAN_POINT ( 'NONE',  ( 9.026838159693451047, 41.84773111872319618, 78.13669174070733447 ) ) ;
#1720 = ORIENTED_EDGE ( 'NONE', *, *, #8592, .T. ) ;
#1721 = ORIENTED_EDGE ( 'NONE', *, *, #6470, .F. ) ;
#1723 = VECTOR ( 'NONE', #10551, 1000.000000000000000 ) ;
#1722 = CARTESIAN_POINT ( 'NONE',  ( 6.447530045045036573, 38.50024170171982973, 76.65924029158320252 ) ) ;
#1724 = CARTESIAN_POINT ( 'NONE',  ( 11.22215374030650281, 42.96218137147968008, 73.80433879953100984 ) ) ;
#1725 = CARTESIAN_POINT ( 'NONE',  ( 7.680615469065380729, 40.16262800804438626, 77.93428071991040440 ) ) ;
#1726 = DIRECTION ( 'NONE',  ( -1.540237394707284220E-16, -1.793354297423764243E-16, 1.000000000000000000 ) ) ;
#1727 = ADVANCED_FACE ( 'NONE', ( #19497 ), #6471, .T. ) ;
#1728 = CARTESIAN_POINT ( 'NONE',  ( 4.713600934472623294, 47.15680210796202232, 92.45433879953098710 ) ) ;
#1729 = ORIENTED_EDGE ( 'NONE', *, *, #17649, .T. ) ;
#1730 = CARTESIAN_POINT ( 'NONE',  ( -4.385374315297738690, 51.47121371654639432, 78.59092584394873882 ) ) ;
#1731 = EDGE_CURVE ( 'NONE', #2631, #8069, #7143, .T. ) ;
#1732 = ORIENTED_EDGE ( 'NONE', *, *, #8303, .F. ) ;
#1733 = CARTESIAN_POINT ( 'NONE',  ( 1.352400422481993658, 50.46853102219002096, 90.57058880123798872 ) ) ;
#1734 = AXIS2_PLACEMENT_3D ( 'NONE', #16275, #19457, #9588 ) ;
#1735 = CARTESIAN_POINT ( 'NONE',  ( 1.257148372430989092, 52.94703067912596595, 76.78082255713043480 ) ) ;
#1736 = CARTESIAN_POINT ( 'NONE',  ( 5.053692675489761754, 42.04909006277621586, 94.82933879611698558 ) ) ;
#1737 = CARTESIAN_POINT ( 'NONE',  ( 8.299662904660788598, 41.56403757284476796, 75.97198585835440099 ) ) ;
#1738 = B_SPLINE_SURFACE_WITH_KNOTS ( 'NONE', 3, 1, ( 
 ( #19513, #6419 ),
 ( #4925, #12928 ),
 ( #18390, #16698 ),
 ( #15103, #511 ),
 ( #3811, #10330 ),
 ( #3967, #7161 ),
 ( #1534, #20874 ),
 ( #17700, #16214 ),
 ( #1639, #1752 ),
 ( #19395, #13123 ),
 ( #14719, #3329 ),
 ( #4601, #1430 ),
 ( #8121, #19288 ) ),
 .UNSPECIFIED., .F., .F., .F.,
 ( 4, 1, 1, 1, 1, 1, 1, 1, 1, 1, 4 ),
 ( 2, 2 ),
 ( 0.000000000000000000, 0.08953921432355217702, 0.1742669454086417657, 0.2528767480256390865, 0.3294736160795620483, 0.4632125218299475988, 0.5712501803543521550, 0.6337422670347153675, 0.7254863994935087934, 0.8484041168876338412, 0.9999999999999998890 ),
 ( 0.000000000000000000, 1.000000000000000000 ),
 .UNSPECIFIED. ) ;
#1739 = LINE ( 'NONE', #11735, #7865 ) ;
#1740 = ORIENTED_EDGE ( 'NONE', *, *, #8730, .T. ) ;
#1741 = ORIENTED_EDGE ( 'NONE', *, *, #5248, .F. ) ;
#1742 = B_SPLINE_CURVE_WITH_KNOTS ( 'NONE', 3,
 ( #15260, #15687, #20236, #10601, #8885, #1108, #2384, #14080, #3965, #20562, #17070, #2495, #10491, #679, #7158, #5987, #13660, #20134, #5569, #9308, #3002, #14491, #1412, #13009, #16097, #9404, #4687 ),
 .UNSPECIFIED., .F., .F.,
 ( 4, 1, 1, 1, 1, 1, 1, 1, 1, 1, 1, 1, 1, 1, 1, 1, 1, 1, 1, 1, 1, 1, 1, 1, 4 ),
 ( 0.000000000000000000, 0.06156270711109813193, 0.1195928175617291256, 0.1747495234496604655, 0.2265549029623682431, 0.2754357869405233972, 0.3212504303641821046, 0.3646692690278454108, 0.4055209537250142326, 0.4439801712034092684, 0.4803226396643038298, 0.5144678959723257838, 0.5464657104125147935, 0.5769957197620103617, 0.6058640933454703115, 0.6335754242279014736, 0.6604510950290067850, 0.6887476664015759198, 0.7209157586619387992, 0.7570169132788651112, 0.7970502319830404803, 0.8414026928090143631, 0.8898175437432860324, 0.9426652073923825759, 1.000000000000000000 ),
 .UNSPECIFIED. ) ;
#1743 = CARTESIAN_POINT ( 'NONE',  ( 28.43948732994508077, 45.16218137147969003, 76.90433879953101837 ) ) ;
#1744 = DIRECTION ( 'NONE',  ( 4.142850521348544074E-16, -5.922860397471813007E-17, 1.000000000000000000 ) ) ;
#1745 = FACE_OUTER_BOUND ( 'NONE', #15464, .T. ) ;
#1746 = ORIENTED_EDGE ( 'NONE', *, *, #3507, .T. ) ;
#1747 = CARTESIAN_POINT ( 'NONE',  ( 1.227438297423749880, 52.33307690334542173, 76.77372445804466849 ) ) ;
#1748 = LINE ( 'NONE', #9729, #14028 ) ;
#1749 = DIRECTION ( 'NONE',  ( 0.3165065846431827645, 0.9485903129789529098, 0.000000000000000000 ) ) ;
#1750 = CARTESIAN_POINT ( 'NONE',  ( 13.32277635493561974, 51.36218137147968577, 93.55433879953098142 ) ) ;
#1751 = EDGE_CURVE ( 'NONE', #5897, #13415, #979, .T. ) ;
#1752 = CARTESIAN_POINT ( 'NONE',  ( 5.081857000512829181, 37.35152159452039911, 77.60331851759366373 ) ) ;
#1753 = ORIENTED_EDGE ( 'NONE', *, *, #9653, .F. ) ;
#1754 = CARTESIAN_POINT ( 'NONE',  ( -1.123656915330052408, 35.37488560990637865, 76.86610350541323555 ) ) ;
#1755 = CYLINDRICAL_SURFACE ( 'NONE', #5195, 0.9921021478795063464 ) ;
#1756 = ORIENTED_EDGE ( 'NONE', *, *, #20011, .F. ) ;
#1757 = CARTESIAN_POINT ( 'NONE',  ( 4.597613975033692846, 52.09221767063174013, 78.17666347917207759 ) ) ;
#1758 = DIRECTION ( 'NONE',  ( -1.000000000000000000, 4.956352788505161887E-15, 0.000000000000000000 ) ) ;
#1759 = CARTESIAN_POINT ( 'NONE',  ( -4.313560930641144431, 37.53965589074172016, 77.26981739744707056 ) ) ;
#1760 = CARTESIAN_POINT ( 'NONE',  ( 5.928963754087451576, 43.92611494815086814, 93.65746379611699979 ) ) ;
#1761 = VECTOR ( 'NONE', #5116, 1000.000000000000114 ) ;
#1762 = CARTESIAN_POINT ( 'NONE',  ( -5.616286711741428128, 44.43019146960381960, 91.23558879782397923 ) ) ;
#1763 = AXIS2_PLACEMENT_3D ( 'NONE', #4022, #5522, #19976 ) ;
#1764 = CARTESIAN_POINT ( 'NONE',  ( 7.992712741985108060, 47.55532711652816147, 77.53155195043741799 ) ) ;
#1765 = CARTESIAN_POINT ( 'NONE',  ( 5.939788499136119171, 51.10080741576499719, 76.32243632687685420 ) ) ;
#1766 = ORIENTED_EDGE ( 'NONE', *, *, #19143, .F. ) ;
#1767 = CARTESIAN_POINT ( 'NONE',  ( 8.722153740306486824, 36.96218137147968008, 95.05433879953098142 ) ) ;
#1768 = CARTESIAN_POINT ( 'NONE',  ( 5.051595465965247556, 37.34078104729439218, 78.11840496518735222 ) ) ;
#1769 = VERTEX_POINT ( 'NONE', #13647 ) ;
#1770 = CARTESIAN_POINT ( 'NONE',  ( 5.581406744796363562, 50.61539444998253856, 76.90580938776616904 ) ) ;
#1771 = EDGE_CURVE ( 'NONE', #19569, #13327, #8659, .T. ) ;
#1772 = CARTESIAN_POINT ( 'NONE',  ( 11.22215374030649926, 51.36218137147968577, 80.55433879953099563 ) ) ;
#1773 = CARTESIAN_POINT ( 'NONE',  ( -4.677846259693497544, 44.16218137147969003, 77.84651775085080772 ) ) ;
#1774 = ORIENTED_EDGE ( 'NONE', *, *, #8570, .T. ) ;
#1775 = DIRECTION ( 'NONE',  ( 6.308085367188358095E-15, 8.847205979147994320E-31, 1.000000000000000000 ) ) ;
#1776 = CARTESIAN_POINT ( 'NONE',  ( -5.561099455747295472, 37.71522085402569502, 75.56266266290518274 ) ) ;
#1777 = ORIENTED_EDGE ( 'NONE', *, *, #1213, .T. ) ;
#1778 = VECTOR ( 'NONE', #17685, 1000.000000000000000 ) ;
#1779 = DIRECTION ( 'NONE',  ( 0.000000000000000000, 0.000000000000000000, -1.000000000000000000 ) ) ;
#1780 = CARTESIAN_POINT ( 'NONE',  ( 31.22215374030650281, 42.76218137147968434, 72.80433879953100984 ) ) ;
#1781 = CARTESIAN_POINT ( 'NONE',  ( 1.256812508749381774, 49.74246873332880625, 96.11746379953099506 ) ) ;
#1782 = ORIENTED_EDGE ( 'NONE', *, *, #20369, .T. ) ;
#1783 = CARTESIAN_POINT ( 'NONE',  ( -4.517072128342576320, 36.94403992325788977, 76.81463291717793140 ) ) ;
#1784 = CARTESIAN_POINT ( 'NONE',  ( -4.608953993764375312, 37.01190935601762533, 77.97288938838477179 ) ) ;
#1785 = CARTESIAN_POINT ( 'NONE',  ( 4.512269934384613101, 47.81844922806527620, 94.12621379953098710 ) ) ;
#1786 = ORIENTED_EDGE ( 'NONE', *, *, #13000, .F. ) ;
#1787 = CARTESIAN_POINT ( 'NONE',  ( 35.92215374030650565, 51.36218137147967866, 92.39963826115175038 ) ) ;
#1788 = DIRECTION ( 'NONE',  ( 0.3014919283324601351, -0.9534121601185491235, 0.01038605259262642688 ) ) ;
#1789 = DIRECTION ( 'NONE',  ( 1.779391786395883536E-16, 5.922860397471806844E-17, -1.000000000000000000 ) ) ;
#1790 = CARTESIAN_POINT ( 'NONE',  ( -4.567115856812060670, 47.10047254335474065, 94.55496380123798872 ) ) ;
#1791 = CARTESIAN_POINT ( 'NONE',  ( 6.149032746747884026, 50.02141417194002315, 75.57514290624801845 ) ) ;
#1792 = ADVANCED_FACE ( 'NONE', ( #3740 ), #8006, .T. ) ;
#1793 = VECTOR ( 'NONE', #11391, 1000.000000000000000 ) ;
#1794 = CARTESIAN_POINT ( 'NONE',  ( 1.082972178424195242, 52.33928642596643499, 76.77198585835439815 ) ) ;
#1795 = CARTESIAN_POINT ( 'NONE',  ( 4.884665026186969961, 36.46369999710588417, 75.53067132529541539 ) ) ;
#1796 = VECTOR ( 'NONE', #12356, 999.9999999999998863 ) ;
#1797 = CARTESIAN_POINT ( 'NONE',  ( 8.458367304687495647, 40.14398790315176058, 79.09910503406773330 ) ) ;
#1798 = ORIENTED_EDGE ( 'NONE', *, *, #11244, .F. ) ;
#1799 = CYLINDRICAL_SURFACE ( 'NONE', #10885, 6.200000000000000178 ) ;
#1800 = CARTESIAN_POINT ( 'NONE',  ( 9.343936824499609273, 42.79809593351145480, 76.16967972087822147 ) ) ;
#1801 = LINE ( 'NONE', #14865, #91 ) ;
#1802 = ORIENTED_EDGE ( 'NONE', *, *, #14580, .T. ) ;
#1803 = EDGE_CURVE ( 'NONE', #6003, #3218, #4264, .T. ) ;
#1804 = PLANE ( 'NONE',  #15413 ) ;
#1805 = ORIENTED_EDGE ( 'NONE', *, *, #19154, .F. ) ;
#1806 = VECTOR ( 'NONE', #13020, 1000.000000000000000 ) ;
#1807 = AXIS2_PLACEMENT_3D ( 'NONE', #11485, #13282, #395 ) ;
#1808 = DIRECTION ( 'NONE',  ( 0.8660254037844399289, 0.4999999999999977796, 0.000000000000000000 ) ) ;
#1809 = FILL_AREA_STYLE_COLOUR ( '', #9110 ) ;
#1810 = CARTESIAN_POINT ( 'NONE',  ( 5.658108625003792191, 37.01637447524286273, 75.97198585835440099 ) ) ;
#1811 = CYLINDRICAL_SURFACE ( 'NONE', #13006, 5.199999999999999289 ) ;
#1812 = CARTESIAN_POINT ( 'NONE',  ( -1.876873622437039701, 39.01745058958429269, 93.96996379782397923 ) ) ;
#1813 = CARTESIAN_POINT ( 'NONE',  ( 2.263363662449209279, 49.77488197367684819, 94.28606768333811772 ) ) ;
#1814 = CARTESIAN_POINT ( 'NONE',  ( -7.677846259693480668, 38.96218137147968008, 93.55433879953098142 ) ) ;
#1815 = PLANE ( 'NONE',  #12513 ) ;
#1816 = CARTESIAN_POINT ( 'NONE',  ( -4.766817752550178255, 37.12851695549264974, 75.97348137399042400 ) ) ;
#1817 = CARTESIAN_POINT ( 'NONE',  ( -5.784195910403845176, 44.99242805365518194, 92.13308880123798872 ) ) ;
#1818 = ORIENTED_EDGE ( 'NONE', *, *, #1038, .T. ) ;
#1819 = CARTESIAN_POINT ( 'NONE',  ( 0.3329282460686175393, 52.96755673690322652, 76.41414202728766725 ) ) ;
#1820 = AXIS2_PLACEMENT_3D ( 'NONE', #8022, #9735, #16326 ) ;
#1821 = CARTESIAN_POINT ( 'NONE',  ( 8.950841833175557483, 41.61996530703199682, 78.68229860608910542 ) ) ;
#1822 = LINE ( 'NONE', #10016, #13008 ) ;
#1823 = CARTESIAN_POINT ( 'NONE',  ( 2.350558581813030123, 49.87752504164860312, 85.32593395802449265 ) ) ;
#1824 = CARTESIAN_POINT ( 'NONE',  ( 8.392716226808454749, 39.94722745792154939, 76.30598982719874357 ) ) ;
#1825 = ORIENTED_EDGE ( 'NONE', *, *, #15179, .T. ) ;
#1826 = CARTESIAN_POINT ( 'NONE',  ( 6.445708703230327963, 38.49894023754261241, 76.49840989696882332 ) ) ;
#1827 = CARTESIAN_POINT ( 'NONE',  ( -0.01650830115698442499, 52.97261345168382007, 79.48573486738433758 ) ) ;
#1828 = CARTESIAN_POINT ( 'NONE',  ( 0.5221537403065114047, 44.16218137147969713, 45.55433879953100273 ) ) ;
#1829 = CARTESIAN_POINT ( 'NONE',  ( -3.522342774269682675, 36.20927341954680401, 76.21065298426071877 ) ) ;
#1830 = CARTESIAN_POINT ( 'NONE',  ( 0.5753667321910650445, 52.96202048236657589, 75.97198585835440099 ) ) ;
#1831 = ORIENTED_EDGE ( 'NONE', *, *, #20566, .F. ) ;
#1832 = CARTESIAN_POINT ( 'NONE',  ( 8.333395564809045197, 41.68949534966480996, 76.00786757613292366 ) ) ;
#1833 = AXIS2_PLACEMENT_3D ( 'NONE', #12926, #16442, #9742 ) ;
#1834 = EDGE_LOOP ( 'NONE', ( #17200, #10352, #12724, #6542 ) ) ;
#1835 = CARTESIAN_POINT ( 'NONE',  ( 6.198496396448986090, 45.68315280215533392, 90.33621380123798872 ) ) ;
#1836 = EDGE_CURVE ( 'NONE', #15570, #468, #4368, .T. ) ;
#1837 = CARTESIAN_POINT ( 'NONE',  ( 2.113017254819833379, 52.20161731206520273, 77.68224048311739693 ) ) ;
#1838 = DIRECTION ( 'NONE',  ( 1.000000000000000000, 1.402518428993831676E-16, 0.000000000000000000 ) ) ;
#1839 = ADVANCED_FACE ( 'NONE', ( #14066 ), #1197, .F. ) ;
#1840 = DIRECTION ( 'NONE',  ( 0.000000000000000000, 0.000000000000000000, -1.000000000000000000 ) ) ;
#1841 = VERTEX_POINT ( 'NONE', #4575 ) ;
#1842 = EDGE_CURVE ( 'NONE', #10155, #10333, #4039, .T. ) ;
#1843 = CARTESIAN_POINT ( 'NONE',  ( 9.353817388681445522, 42.82770861117572281, 76.74257409364852833 ) ) ;
#1844 = EDGE_LOOP ( 'NONE', ( #10122, #11352, #17562, #17623 ) ) ;
#1845 = CARTESIAN_POINT ( 'NONE',  ( -7.423951210289297720, 47.94363824867885171, 78.32492703482499508 ) ) ;
#1846 = CARTESIAN_POINT ( 'NONE',  ( 3.212180877488374886, 51.27651577472676792, 72.45433879953087342 ) ) ;
#1847 = CARTESIAN_POINT ( 'NONE',  ( -5.784195910403845176, 44.99242805365518194, 95.88308880123798872 ) ) ;
#1848 = EDGE_CURVE ( 'NONE', #17827, #15970, #19163, .T. ) ;
#1849 = ORIENTED_EDGE ( 'NONE', *, *, #6078, .T. ) ;
#1850 = LINE ( 'NONE', #3847, #13372 ) ;
#1851 = CARTESIAN_POINT ( 'NONE',  ( -4.811608766808348037, 37.16160227343304712, 79.54845644658969661 ) ) ;
#1852 = CARTESIAN_POINT ( 'NONE',  ( 5.921589662822362321, 51.11425016305613411, 76.13071926429850578 ) ) ;
#1853 = CARTESIAN_POINT ( 'NONE',  ( -1.477846259693491149, 49.81903562097206617, 123.5543387995310098 ) ) ;
#1854 = VERTEX_POINT ( 'NONE', #17363 ) ;
#1855 = CARTESIAN_POINT ( 'NONE',  ( 31.03948732994507864, 43.16218137147969003, 77.50433879953099847 ) ) ;
#1856 = ORIENTED_EDGE ( 'NONE', *, *, #9229, .T. ) ;
#1857 = CARTESIAN_POINT ( 'NONE',  ( 4.355143591211044551, 51.35730577063056046, 77.83360891957636341 ) ) ;
#1858 = CARTESIAN_POINT ( 'NONE',  ( -6.705246719490330243, 40.29814987666313186, 78.47931198110067896 ) ) ;
#1859 = FACE_OUTER_BOUND ( 'NONE', #20961, .T. ) ;
#1860 = CARTESIAN_POINT ( 'NONE',  ( 2.635245049009969254, 48.69372030666295359, 92.64183879611699979 ) ) ;
#1861 = DIRECTION ( 'NONE',  ( 0.5800177190770278157, 0.8146038580541354879, 2.354238310054624259E-16 ) ) ;
#1862 = LINE ( 'NONE', #16443, #15009 ) ;
#1863 = DIRECTION ( 'NONE',  ( -1.402518428993831183E-16, 1.000000000000000000, -3.469446951953617640E-16 ) ) ;
#1864 = B_SPLINE_CURVE_WITH_KNOTS ( 'NONE', 3,
 ( #14878, #17971, #16176, #19350, #16487, #16276, #14777, #100, #1707, #6579 ),
 .UNSPECIFIED., .F., .F.,
 ( 4, 2, 2, 2, 4 ),
 ( 0.000000000000000000, 0.0002556600934737911549, 0.0005113201869475823098, 0.0007669802804213734105, 0.001022640373895164620 ),
 .UNSPECIFIED. ) ;
#1865 = ORIENTED_EDGE ( 'NONE', *, *, #2067, .T. ) ;
#1866 = EDGE_CURVE ( 'NONE', #3490, #18561, #4520, .T. ) ;
#1867 = CARTESIAN_POINT ( 'NONE',  ( 5.231589412277350526, 37.46939813133004549, 78.26671861549210973 ) ) ;
#1868 = VERTEX_POINT ( 'NONE', #9603 ) ;
#1869 = CARTESIAN_POINT ( 'NONE',  ( 31.22215374030650281, 42.96218137147968008, 73.80433879953100984 ) ) ;
#1870 = CARTESIAN_POINT ( 'NONE',  ( -1.306251101200015752, 49.87752504164858891, 85.32593395802449265 ) ) ;
#1871 = CARTESIAN_POINT ( 'NONE',  ( 3.948530577815480225, 39.69684013992245752, 95.64871379953100927 ) ) ;
#1872 = VERTEX_POINT ( 'NONE', #10998 ) ;
#1873 = CARTESIAN_POINT ( 'NONE',  ( -4.524181921268124462, 40.28999182795290324, 96.19558880123798872 ) ) ;
#1874 = CARTESIAN_POINT ( 'NONE',  ( -5.113776628078608333, 38.32080799658261583, 75.56266266290518274 ) ) ;
#1875 = ORIENTED_EDGE ( 'NONE', *, *, #2222, .F. ) ;
#1876 = CARTESIAN_POINT ( 'NONE',  ( 5.753005855668248181, 51.23877623043087937, 78.93669174070734584 ) ) ;
#1877 = CARTESIAN_POINT ( 'NONE',  ( 0.3548969944630057660, 52.96060458516934233, 76.08537024512065727 ) ) ;
#1878 = CARTESIAN_POINT ( 'NONE',  ( -5.058133621542618030, 44.89684013992257405, 95.17996379953099506 ) ) ;
#1879 = VERTEX_POINT ( 'NONE', #17469 ) ;
#1880 = DIRECTION ( 'NONE',  ( -0.000000000000000000, -0.000000000000000000, 1.000000000000000000 ) ) ;
#1881 = ORIENTED_EDGE ( 'NONE', *, *, #9105, .T. ) ;
#1882 = DIRECTION ( 'NONE',  ( -3.893792155548169402E-16, -7.183611964723547524E-17, 1.000000000000000000 ) ) ;
#1883 = CARTESIAN_POINT ( 'NONE',  ( 5.426454583374004770, 50.73403188498316041, 78.93531119083770875 ) ) ;
#1884 = CARTESIAN_POINT ( 'NONE',  ( 2.263363662449209279, 49.77488197367684819, 94.28606768333811772 ) ) ;
#1885 = CARTESIAN_POINT ( 'NONE',  ( 4.394343283833276992, 39.11584570990505938, 93.85183880123797451 ) ) ;
#1886 = DIRECTION ( 'NONE',  ( 1.000000000000000000, 0.000000000000000000, 0.000000000000000000 ) ) ;
#1887 = CARTESIAN_POINT ( 'NONE',  ( 5.963693060521315203, 51.08315007920423056, 75.36814786694185386 ) ) ;
#1888 = PLANE ( 'NONE',  #16052 ) ;
#1889 = CARTESIAN_POINT ( 'NONE',  ( 5.471341376803050771, 36.88291743766401254, 75.36841521003546518 ) ) ;
#1890 = CARTESIAN_POINT ( 'NONE',  ( 8.385938212755766230, 39.92691331981644254, 77.86095545630369941 ) ) ;
#1891 = EDGE_LOOP ( 'NONE', ( #6937, #16639, #1239, #20060 ) ) ;
#1892 = DIRECTION ( 'NONE',  ( -1.540237394707284220E-16, -1.793354297423764243E-16, 1.000000000000000000 ) ) ;
#1893 = CARTESIAN_POINT ( 'NONE',  ( 9.332226353535185481, 42.76299890913265500, 76.00948821603452643 ) ) ;
#1894 = CARTESIAN_POINT ( 'NONE',  ( -5.888748219722875987, 40.55551840971140365, 78.50801527011910252 ) ) ;
#1895 = PLANE ( 'NONE',  #19754 ) ;
#1896 = EDGE_LOOP ( 'NONE', ( #13114, #18259, #1616, #5276 ) ) ;
#1897 = ORIENTED_EDGE ( 'NONE', *, *, #18926, .F. ) ;
#1898 = CARTESIAN_POINT ( 'NONE',  ( 5.544276951911416340, 50.64433212932689088, 78.59183879953087626 ) ) ;
#1899 = EDGE_LOOP ( 'NONE', ( #5010, #17264, #11538, #20190 ) ) ;
#1900 = CARTESIAN_POINT ( 'NONE',  ( -3.752498811055295924, 36.37928041266965806, 77.59103917682324436 ) ) ;
#1901 = EDGE_CURVE ( 'NONE', #10941, #9206, #18999, .T. ) ;
#1902 = FACE_OUTER_BOUND ( 'NONE', #6911, .T. ) ;
#1903 = FACE_OUTER_BOUND ( 'NONE', #5735, .T. ) ;
#1904 = CARTESIAN_POINT ( 'NONE',  ( -0.6408505906039995148, 52.88534186852020014, 75.73072098668157537 ) ) ;
#1905 = CARTESIAN_POINT ( 'NONE',  ( 28.52215374030649642, 44.16218137147969003, 87.85433879953103542 ) ) ;
#1906 = CARTESIAN_POINT ( 'NONE',  ( 4.119841024906783389, 51.52029635603552293, 76.17419329630023128 ) ) ;
#1907 = CARTESIAN_POINT ( 'NONE',  ( -3.510185363184280316, 36.20029322970840724, 76.30596599901106458 ) ) ;
#1908 = CARTESIAN_POINT ( 'NONE',  ( 6.198496396448986090, 45.68315280215533392, 94.08621380123798872 ) ) ;
#1909 = CARTESIAN_POINT ( 'NONE',  ( -4.567115856812060670, 47.10047254335474065, 92.05496380123798872 ) ) ;
#1910 = ORIENTED_EDGE ( 'NONE', *, *, #11885, .T. ) ;
#1911 = CARTESIAN_POINT ( 'NONE',  ( 4.045888121501547197, 36.75785668915397508, 76.03652549193961363 ) ) ;
#1912 = FACE_OUTER_BOUND ( 'NONE', #18202, .T. ) ;
#1913 = CARTESIAN_POINT ( 'NONE',  ( 5.362953798781178172, 50.78084096341162024, 78.93369693484829952 ) ) ;
#1914 = CARTESIAN_POINT ( 'NONE',  ( 0.3201111382462867860, 51.36399839264385037, 77.10139762306027933 ) ) ;
#1915 = DIRECTION ( 'NONE',  ( -0.9485903129789527988, 0.3165065846431829311, -8.934458285744989980E-17 ) ) ;
#1916 = ORIENTED_EDGE ( 'NONE', *, *, #20288, .F. ) ;
#1917 = EDGE_CURVE ( 'NONE', #2886, #14804, #14891, .T. ) ;
#1918 = CARTESIAN_POINT ( 'NONE',  ( 9.353817388681445522, 42.82770861117572281, 77.06316232894263862 ) ) ;
#1919 = CARTESIAN_POINT ( 'NONE',  ( 8.004281444754417052, 40.80494971592259645, 79.42365263778002316 ) ) ;
#1920 = CARTESIAN_POINT ( 'NONE',  ( -3.815104224344752382, 36.42552450956669929, 75.61442449207443417 ) ) ;
#1921 = CARTESIAN_POINT ( 'NONE',  ( 5.421101980426652922, 50.73801848575102014, 77.95022289312436214 ) ) ;
#1922 = EDGE_LOOP ( 'NONE', ( #4715, #10698, #8890, #840, #7355, #19426 ) ) ;
#1923 = CARTESIAN_POINT ( 'NONE',  ( 8.921551879414991504, 41.53218145749156776, 76.03029119948048731 ) ) ;
#1924 = AXIS2_PLACEMENT_3D ( 'NONE', #17258, #5973, #1295 ) ;
#1925 = DIRECTION ( 'NONE',  ( 1.000000000000000000, 0.000000000000000000, 0.000000000000000000 ) ) ;
#1926 = EDGE_LOOP ( 'NONE', ( #18975, #6201, #1697, #9756 ) ) ;
#1927 = CARTESIAN_POINT ( 'NONE',  ( 1.868012774839550749, 39.13936707477651566, 94.63308880294498238 ) ) ;
#1928 = DIRECTION ( 'NONE',  ( 1.779391786395883536E-16, 5.922860397471806844E-17, -1.000000000000000000 ) ) ;
#1929 = B_SPLINE_CURVE_WITH_KNOTS ( 'NONE', 3,
 ( #20504, #19125, #4439, #9138, #17112, #10853, #7640, #2637, #2948, #14121, #2535, #17425, #1047, #20603, #2850, #9030, #15517, #12330, #6031 ),
 .UNSPECIFIED., .F., .F.,
 ( 4, 1, 1, 1, 1, 1, 1, 1, 1, 1, 1, 1, 1, 1, 1, 1, 4 ),
 ( 0.000000000000000000, 0.1026547437176949656, 0.1953110930976798554, 0.2773242249590897601, 0.3493914542831295655, 0.4108068724308638342, 0.4622887491528899773, 0.5032980238437735343, 0.5345418472720404601, 0.5847168530758872773, 0.6322731508218554231, 0.6775315938118185999, 0.7246750034944897667, 0.7779009386454487363, 0.8408031781967141294, 0.9146367246678260843, 1.000000000000000000 ),
 .UNSPECIFIED. ) ;
#1930 = EDGE_CURVE ( 'NONE', #5867, #13124, #19678, .T. ) ;
#1931 = CARTESIAN_POINT ( 'NONE',  ( 5.146043734657006041, 40.41782908280415398, 90.30634084312077903 ) ) ;
#1932 = EDGE_CURVE ( 'NONE', #667, #19622, #16292, .T. ) ;
#1933 = DIRECTION ( 'NONE',  ( 0.007885122365275663500, 0.9999689119394085113, 1.805443505845543142E-16 ) ) ;
#1934 = ORIENTED_EDGE ( 'NONE', *, *, #1069, .F. ) ;
#1935 = LINE ( 'NONE', #6926, #20960 ) ;
#1936 = ORIENTED_EDGE ( 'NONE', *, *, #9256, .F. ) ;
#1937 = CARTESIAN_POINT ( 'NONE',  ( -7.519011464410084500, 47.73881877701913368, 78.32326252082832241 ) ) ;
#1938 = EDGE_CURVE ( 'NONE', #10995, #17381, #4616, .T. ) ;
#1939 = DIRECTION ( 'NONE',  ( 0.007885122365275663500, 0.9999689119394085113, 1.805443505845543142E-16 ) ) ;
#1940 = ORIENTED_EDGE ( 'NONE', *, *, #14592, .F. ) ;
#1941 = EDGE_CURVE ( 'NONE', #9093, #14083, #18312, .T. ) ;
#1942 = CARTESIAN_POINT ( 'NONE',  ( 5.591308205070053994, 40.32050054405898720, 54.55433879953099563 ) ) ;
#1943 = EDGE_CURVE ( 'NONE', #20669, #9230, #12884, .T. ) ;
#1944 = CARTESIAN_POINT ( 'NONE',  ( 8.059489980808651310, 41.32971201870342526, 75.37437276336991943 ) ) ;
#1945 = CARTESIAN_POINT ( 'NONE',  ( -5.667418469993653396, 43.80274312437727247, 78.25433879953087057 ) ) ;
#1946 = CARTESIAN_POINT ( 'NONE',  ( -7.677846259693483333, 47.36218137147966445, 93.55433879953098142 ) ) ;
#1947 = ADVANCED_FACE ( 'NONE', ( #13099 ), #17687, .F. ) ;
#1948 = CARTESIAN_POINT ( 'NONE',  ( -4.176309363623030180, 42.45208065485131499, 93.42308879953097289 ) ) ;
#1949 = ORIENTED_EDGE ( 'NONE', *, *, #13892, .F. ) ;
#1950 = CARTESIAN_POINT ( 'NONE',  ( -4.486751758304120763, 51.39877310743911210, 75.98707017319573254 ) ) ;
#1951 = ORIENTED_EDGE ( 'NONE', *, *, #10188, .T. ) ;
#1952 = CARTESIAN_POINT ( 'NONE',  ( 1.855487073639847218, 49.49551470481303284, 77.82100546619766135 ) ) ;
#1953 = CARTESIAN_POINT ( 'NONE',  ( -6.705008690618248224, 40.29739715461727201, 78.50801527011910252 ) ) ;
#1954 = EDGE_CURVE ( 'NONE', #20010, #15290, #19843, .T. ) ;
#1955 = DIRECTION ( 'NONE',  ( 0.000000000000000000, 1.000000000000000000, 0.000000000000000000 ) ) ;
#1956 = CARTESIAN_POINT ( 'NONE',  ( 6.924055141134583202, 50.37376929599953712, 78.48669174070734300 ) ) ;
#1957 = PLANE ( 'NONE',  #20657 ) ;
#1958 = CARTESIAN_POINT ( 'NONE',  ( -4.622577041588895597, 46.56120873422322859, 91.31371379782397923 ) ) ;
#1959 = CARTESIAN_POINT ( 'NONE',  ( 2.392664886727889240, 47.70104341108813628, 61.28382765310962554 ) ) ;
#1960 =( BOUNDED_CURVE ( )  B_SPLINE_CURVE ( 3, ( #18246, #5048, #8468, #3568 ),
 .UNSPECIFIED., .F., .T. ) 
 B_SPLINE_CURVE_WITH_KNOTS ( ( 4, 4 ),
 ( 5.006904465492826972, 5.052225889838810602 ),
 .UNSPECIFIED. ) 
 CURVE ( )  GEOMETRIC_REPRESENTATION_ITEM ( )  RATIONAL_B_SPLINE_CURVE ( ( 1.000000000000000000, 0.9998288380325438540, 0.9998288380325438540, 1.000000000000000000 ) ) 
 REPRESENTATION_ITEM ( '' )  );
#1961 = CARTESIAN_POINT ( 'NONE',  ( -7.712300854543705952, 47.28237451121256640, 78.18191347276355430 ) ) ;
#1962 = ORIENTED_EDGE ( 'NONE', *, *, #9217, .F. ) ;
#1963 = CARTESIAN_POINT ( 'NONE',  ( 0.8357988670611854465, 52.21160558265095375, 79.54553221853565503 ) ) ;
#1964 = DIRECTION ( 'NONE',  ( 1.110223024625156540E-16, 1.000000000000000000, 5.922860397471808077E-17 ) ) ;
#1965 = B_SPLINE_CURVE_WITH_KNOTS ( 'NONE', 3,
 ( #19750, #5273, #16681, #5171, #15182, #20061, #12206, #15506, #14009, #7303, #9124, #5814, #5599, #18583, #6018, #1031 ),
 .UNSPECIFIED., .F., .F.,
 ( 4, 2, 2, 2, 2, 2, 2, 4 ),
 ( 0.000000000000000000, 0.0007061632881199156157, 0.0008827041101498631862, 0.001059244932179810757, 0.001412326576239666650, 0.001765408220299522542, 0.002118489864359378218, 0.002824653152479090004 ),
 .UNSPECIFIED. ) ;
#1966 = VECTOR ( 'NONE', #12254, 1000.000000000000227 ) ;
#1967 = ORIENTED_EDGE ( 'NONE', *, *, #10805, .T. ) ;
#1968 = CARTESIAN_POINT ( 'NONE',  ( 7.691771551572207599, 40.18266124458227750, 75.45433879953088763 ) ) ;
#1969 = FACE_OUTER_BOUND ( 'NONE', #8698, .T. ) ;
#1970 = CARTESIAN_POINT ( 'NONE',  ( 5.025485839985549319, 41.56218137147963887, 91.97683879953100927 ) ) ;
#1971 = ORIENTED_EDGE ( 'NONE', *, *, #11662, .F. ) ;
#1972 = PRESENTATION_STYLE_ASSIGNMENT (( #19731 ) ) ;
#1973 = CARTESIAN_POINT ( 'NONE',  ( -5.907462774012225637, 37.97106548486248556, 76.06004113464240390 ) ) ;
#1974 = ORIENTED_EDGE ( 'NONE', *, *, #2689, .F. ) ;
#1975 = DIRECTION ( 'NONE',  ( 2.043266227890062685E-16, 0.7071067811865451302, -0.7071067811865500152 ) ) ;
#1976 = CARTESIAN_POINT ( 'NONE',  ( 0.4461516307629347367, 52.96189878203579582, 76.96012881851619625 ) ) ;
#1977 = EDGE_CURVE ( 'NONE', #8963, #10468, #19137, .T. ) ;
#1978 = CARTESIAN_POINT ( 'NONE',  ( -2.904223097202481174, 48.62752260303690122, 92.52371379953099506 ) ) ;
#1979 = ORIENTED_EDGE ( 'NONE', *, *, #9383, .T. ) ;
#1980 = LINE ( 'NONE', #6758, #8511 ) ;
#1981 = EDGE_LOOP ( 'NONE', ( #9342, #8226, #9610, #11212 ) ) ;
#1982 = CARTESIAN_POINT ( 'NONE',  ( -4.795362370604993707, 51.17825126284458293, 76.19771883405211099 ) ) ;
#1983 = CARTESIAN_POINT ( 'NONE',  ( 2.578515286158505670, 49.45973034996755047, 94.15269390996789411 ) ) ;
#1984 = ADVANCED_FACE ( 'NONE', ( #6041 ), #16158, .F. ) ;
#1985 = VECTOR ( 'NONE', #11567, 1000.000000000000114 ) ;
#1986 = CARTESIAN_POINT ( 'NONE',  ( -0.05922600882914304254, 0.000000000000000000, -8.198594120679954855 ) ) ;
#1987 = CARTESIAN_POINT ( 'NONE',  ( 5.712959422672630794, 50.34352397032943571, 75.39427037473855364 ) ) ;
#1988 = CARTESIAN_POINT ( 'NONE',  ( 5.433321616587456049, 50.72893591270732827, 77.28832074152185783 ) ) ;
#1989 = CARTESIAN_POINT ( 'NONE',  ( -3.479253321868470916, 37.00426859223156129, 79.33569596569910232 ) ) ;
#1990 = EDGE_CURVE ( 'NONE', #1268, #19018, #9262, .T. ) ;
#1991 = CARTESIAN_POINT ( 'NONE',  ( 4.393996117251955269, 36.11308595931626542, 76.73963291717792856 ) ) ;
#1992 = CARTESIAN_POINT ( 'NONE',  ( 8.496565932950701949, 40.25847161533236829, 79.21682452846883393 ) ) ;
#1993 = ORIENTED_EDGE ( 'NONE', *, *, #6250, .T. ) ;
#1994 = CARTESIAN_POINT ( 'NONE',  ( 0.5221537403065019678, 44.16218137147968292, 72.45433879953087342 ) ) ;
#1995 = CARTESIAN_POINT ( 'NONE',  ( 9.115819689944924420, 42.11441440976988559, 75.45386443748748206 ) ) ;
#1996 = CARTESIAN_POINT ( 'NONE',  ( 2.643026689701002407, 51.46641972551267941, 72.45433879953087342 ) ) ;
#1997 = CARTESIAN_POINT ( 'NONE',  ( 4.394343283833276992, 39.11584570990505938, 95.25808880123800293 ) ) ;
#1998 = ORIENTED_EDGE ( 'NONE', *, *, #1803, .T. ) ;
#1999 = VECTOR ( 'NONE', #2801, 1000.000000000000000 ) ;
#2000 = VERTEX_POINT ( 'NONE', #1166 ) ;
#2001 = CARTESIAN_POINT ( 'NONE',  ( 5.902048492000326441, 51.12868443877599134, 78.59183879953087626 ) ) ;
#2002 = ORIENTED_EDGE ( 'NONE', *, *, #15969, .T. ) ;
#2003 = CARTESIAN_POINT ( 'NONE',  ( 5.581406744796362673, 50.61539444998253856, 76.38301527011910252 ) ) ;
#2004 = DIRECTION ( 'NONE',  ( -0.000000000000000000, 0.000000000000000000, -1.000000000000000000 ) ) ;
#2005 = CARTESIAN_POINT ( 'NONE',  ( 4.629792079547915939, 52.06844900104020013, 77.37197156638603701 ) ) ;
#2006 = CARTESIAN_POINT ( 'NONE',  ( -2.582283693828128168, 37.50405593653111680, 78.46683879953087626 ) ) ;
#2007 = CARTESIAN_POINT ( 'NONE',  ( 35.92215374030650565, 40.96218137147972982, 45.55433879953098852 ) ) ;
#2008 = CARTESIAN_POINT ( 'NONE',  ( 8.787869161997047485, 41.13152587271654426, 76.34522901481825841 ) ) ;
#2009 = DIRECTION ( 'NONE',  ( -3.211742425186504723E-16, 5.922860397471811774E-17, -1.000000000000000000 ) ) ;
#2010 = PLANE ( 'NONE',  #6118 ) ;
#2011 = CARTESIAN_POINT ( 'NONE',  ( -0.9988176903691428077, 49.83852402762217082, 93.14871380123798872 ) ) ;
#2012 = VECTOR ( 'NONE', #19910, 1000.000000000000000 ) ;
#2013 = CARTESIAN_POINT ( 'NONE',  ( 5.568489401881125289, 48.03437091500646261, 90.41433880123798872 ) ) ;
#2014 = ORIENTED_EDGE ( 'NONE', *, *, #1029, .T. ) ;
#2015 = CARTESIAN_POINT ( 'NONE',  ( 0.3467105299092503312, 52.96744805853006710, 76.10778090364108550 ) ) ;
#2016 = AXIS2_PLACEMENT_3D ( 'NONE', #14834, #16545, #8247 ) ;
#2017 = CARTESIAN_POINT ( 'NONE',  ( 0.5221537403065019678, 44.16218137147968292, 72.45433879953087342 ) ) ;
#2018 = CARTESIAN_POINT ( 'NONE',  ( -5.721665869871382704, 50.51634869640449210, 78.97495844722888592 ) ) ;
#2019 = CARTESIAN_POINT ( 'NONE',  ( 8.432571228970111576, 41.99999248199843294, 75.38373313750008720 ) ) ;
#2020 = CARTESIAN_POINT ( 'NONE',  ( 2.043125170982144745, 38.48583871533720213, 92.67996380123798872 ) ) ;
#2021 = VECTOR ( 'NONE', #15116, 1000.000000000000000 ) ;
#2022 = CARTESIAN_POINT ( 'NONE',  ( 8.374750565220676179, 41.81343890941077746, 77.24172240072661566 ) ) ;
#2023 = DIRECTION ( 'NONE',  ( 2.043266227890062685E-16, 0.7071067811865451302, -0.7071067811865500152 ) ) ;
#2024 = CARTESIAN_POINT ( 'NONE',  ( 5.722153871299536121, 42.76884579772442407, 93.58987682607209990 ) ) ;
#2025 = ORIENTED_EDGE ( 'NONE', *, *, #9304, .F. ) ;
#2026 = ORIENTED_EDGE ( 'NONE', *, *, #9076, .F. ) ;
#2027 = AXIS2_PLACEMENT_3D ( 'NONE', #12596, #18970, #11112 ) ;
#2028 = B_SPLINE_CURVE_WITH_KNOTS ( 'NONE', 3,
 ( #2140, #433, #530, #3413, #8641, #18198, #1921, #16408 ),
 .UNSPECIFIED., .F., .F.,
 ( 4, 2, 2, 4 ),
 ( 0.000000000000000000, 0.0002181616706891221331, 0.0003272425060336631554, 0.0004363233413782042591 ),
 .UNSPECIFIED. ) ;
#2029 = CARTESIAN_POINT ( 'NONE',  ( 9.335797811945472091, 42.77370279655738017, 78.83313045764568017 ) ) ;
#2030 = LINE ( 'NONE', #6594, #13481 ) ;
#2031 = DIRECTION ( 'NONE',  ( 0.000000000000000000, 0.000000000000000000, -1.000000000000000000 ) ) ;
#2032 = VERTEX_POINT ( 'NONE', #20712 ) ;
#2033 = DIRECTION ( 'NONE',  ( 1.000000000000000000, 0.000000000000000000, 0.000000000000000000 ) ) ;
#2034 = AXIS2_PLACEMENT_3D ( 'NONE', #11051, #6028, #19216 ) ;
#2035 = DIRECTION ( 'NONE',  ( 6.308085367188358884E-15, 3.469446951953626515E-16, 1.000000000000000000 ) ) ;
#2036 = EDGE_LOOP ( 'NONE', ( #17023, #19666, #5561, #5661, #11166, #11199 ) ) ;
#2037 = CARTESIAN_POINT ( 'NONE',  ( -4.500660556396669065, 42.81632233694663370, 94.32058880294496817 ) ) ;
#2038 = CARTESIAN_POINT ( 'NONE',  ( 1.874180992794621803, 52.20350062376504496, 77.04052575557504667 ) ) ;
#2039 = EDGE_CURVE ( 'NONE', #16740, #7726, #5055, .T. ) ;
#2040 = CARTESIAN_POINT ( 'NONE',  ( -0.3080929418689875576, 37.85583172076933778, 91.35183880123798872 ) ) ;
#2041 = VECTOR ( 'NONE', #13553, 1000.000000000000114 ) ;
#2042 = DIRECTION ( 'NONE',  ( 5.213532094855085691E-33, -3.469446951953617640E-16, -1.000000000000000000 ) ) ;
#2043 = ORIENTED_EDGE ( 'NONE', *, *, #5556, .T. ) ;
#2044 = CARTESIAN_POINT ( 'NONE',  ( 23.03948732994508575, 45.16218137147969003, 73.00433879953099847 ) ) ;
#2045 = ORIENTED_EDGE ( 'NONE', *, *, #14164, .T. ) ;
#2046 = AXIS2_PLACEMENT_3D ( 'NONE', #12940, #1662, #7943 ) ;
#2047 = CARTESIAN_POINT ( 'NONE',  ( -7.723575267056036253, 47.23593929668128766, 77.80994480216610043 ) ) ;
#2048 = CARTESIAN_POINT ( 'NONE',  ( 5.568489401881125289, 48.03437091500646261, 91.66433880123796030 ) ) ;
#2049 = EDGE_LOOP ( 'NONE', ( #19952, #16557 ) ) ;
#2050 = CARTESIAN_POINT ( 'NONE',  ( 8.424733569470319594, 41.97255615673255846, 78.13519505141211141 ) ) ;
#2051 = CARTESIAN_POINT ( 'NONE',  ( 8.677276008184190204, 40.80007117484056067, 75.42295143068700725 ) ) ;
#2052 = CARTESIAN_POINT ( 'NONE',  ( -4.176309363623031068, 42.45208065485131499, 94.67308879953097289 ) ) ;
#2053 = ADVANCED_FACE ( 'NONE', ( #278 ), #9885, .F. ) ;
#2054 = DIRECTION ( 'NONE',  ( 1.000000000000000000, -0.000000000000000000, -0.000000000000000000 ) ) ;
#2055 = CARTESIAN_POINT ( 'NONE',  ( 0.3655949440400476647, 52.96731361127903170, 78.79918605040184332 ) ) ;
#2056 = VERTEX_POINT ( 'NONE', #6768 ) ;
#2057 = CARTESIAN_POINT ( 'NONE',  ( -3.445544706522349454, 39.98463554099927109, 92.55433879953096721 ) ) ;
#2058 = VERTEX_POINT ( 'NONE', #12958 ) ;
#2059 = DIRECTION ( 'NONE',  ( -1.540237394707284220E-16, -1.793354297423764243E-16, 1.000000000000000000 ) ) ;
#2060 = CARTESIAN_POINT ( 'NONE',  ( -7.521768377761679503, 40.39618086641783634, 77.60658645233600339 ) ) ;
#2061 = ADVANCED_FACE ( 'NONE', ( #9991 ), #9375, .T. ) ;
#2062 = PLANE ( 'NONE',  #11553 ) ;
#2063 = CARTESIAN_POINT ( 'NONE',  ( -1.306251101200014197, 49.87752504164859602, 53.32593395802448555 ) ) ;
#2064 = VECTOR ( 'NONE', #13822, 1000.000000000000000 ) ;
#2065 = CARTESIAN_POINT ( 'NONE',  ( 0.7901638384306286511, 50.30062182352762079, 92.32933879782399345 ) ) ;
#2066 = CARTESIAN_POINT ( 'NONE',  ( 5.839584039462725862, 37.14605016217623046, 76.11636564480957645 ) ) ;
#2067 = EDGE_CURVE ( 'NONE', #14315, #18045, #3155, .T. ) ;
#2068 = ORIENTED_EDGE ( 'NONE', *, *, #7854, .T. ) ;
#2069 = FACE_OUTER_BOUND ( 'NONE', #7311, .T. ) ;
#2070 = PRODUCT_DEFINITION_FORMATION_WITH_SPECIFIED_SOURCE ( 'ANY', '', #3597, .NOT_KNOWN. ) ;
#2071 = CARTESIAN_POINT ( 'NONE',  ( 5.831313177393474767, 37.14014010695713353, 78.35708441643889444 ) ) ;
#2072 = ORIENTED_EDGE ( 'NONE', *, *, #12976, .F. ) ;
#2073 = FACE_OUTER_BOUND ( 'NONE', #8920, .T. ) ;
#2074 = EDGE_CURVE ( 'NONE', #17824, #13387, #20801, .T. ) ;
#2075 = CARTESIAN_POINT ( 'NONE',  ( -3.539401246598059991, 43.09270903039240608, 82.45433879953087342 ) ) ;
#2076 = CARTESIAN_POINT ( 'NONE',  ( -0.8237052942265477018, 49.18499566818285018, 94.94558879953099506 ) ) ;
#2077 = B_SPLINE_SURFACE_WITH_KNOTS ( 'NONE', 3, 1, ( 
 ( #5486, #7296 ),
 ( #705, #8298 ),
 ( #5690, #3989 ),
 ( #11607, #15284 ),
 ( #10511, #19663 ),
 ( #16388, #16777 ),
 ( #814, #17972 ),
 ( #12199, #7185 ),
 ( #19560, #18679 ),
 ( #12096, #13686 ),
 ( #12000, #13571 ),
 ( #10626, #3394 ),
 ( #9908, #1816 ),
 ( #18471, #10408 ),
 ( #3783, #17095 ) ),
 .UNSPECIFIED., .F., .F., .F.,
 ( 4, 1, 1, 1, 1, 1, 1, 1, 1, 1, 1, 1, 4 ),
 ( 2, 2 ),
 ( 0.000000000000000000, 0.1167597168375007488, 0.2214683318549902913, 0.3169846747733736647, 0.4005759510517727939, 0.4723184013547362947, 0.5354911787873812834, 0.5872921887835030885, 0.6299408870648134373, 0.7051993628396346914, 0.7869278594151544182, 0.8829706743529757151, 1.000000000000000000 ),
 ( 0.000000000000000000, 1.000000000000000000 ),
 .UNSPECIFIED. ) ;
#2078 = ORIENTED_EDGE ( 'NONE', *, *, #17255, .T. ) ;
#2079 = CARTESIAN_POINT ( 'NONE',  ( -3.350035803220276609, 49.20851703305431357, 95.88308880123798872 ) ) ;
#2080 = CARTESIAN_POINT ( 'NONE',  ( -5.441628559556528799, 38.56297901168398568, 75.98496980016291502 ) ) ;
#2081 = ORIENTED_EDGE ( 'NONE', *, *, #4414, .T. ) ;
#2082 = CARTESIAN_POINT ( 'NONE',  ( 5.404201196092212278, 50.75047497752489534, 79.54845644658969661 ) ) ;
#2083 = CARTESIAN_POINT ( 'NONE',  ( -4.519095118814112411, 36.94553422482819371, 76.36459416792565946 ) ) ;
#2084 = VERTEX_POINT ( 'NONE', #12629 ) ;
#2085 = CARTESIAN_POINT ( 'NONE',  ( -3.055882809522131094, 36.78399362325244937, 72.45433879953085921 ) ) ;
#2086 = CARTESIAN_POINT ( 'NONE',  ( -0.3080929418689875576, 37.85583172076933778, 95.10183880123796030 ) ) ;
#2087 = ORIENTED_EDGE ( 'NONE', *, *, #7762, .F. ) ;
#2088 = LINE ( 'NONE', #484, #12128 ) ;
#2089 = DIRECTION ( 'NONE',  ( -0.3165065846431826535, -0.9485903129789529098, -2.188653791613874008E-16 ) ) ;
#2090 = AXIS2_PLACEMENT_3D ( 'NONE', #3293, #14884, #8405 ) ;
#2091 =( BOUNDED_SURFACE ( )  B_SPLINE_SURFACE ( 1, 2, ( 
 ( #4682, #1515, #11203, #3108, #9611, #20557, #1204, #9400, #2996, #18964, #6080, #10901, #16093, #9303, #8001, #14487, #20954, #9196, #4791, #6389, #7690, #1103, #12891, #15885, #19373, #14272, #7790, #20753, #11313, #2688, #20650, #6186, #15683, #7592, #12585, #11006, #17477, #2903, #12691, #17886, #11732, #6494, #19, #11415, #18203, #3308, #19579, #3418, #17787, #14696, #4895, #3624, #17995, #13212, #3212, #323, #10133, #19687, #9930, #14797, #16194, #5111, #8104, #14900, #13107, #9816, #5313, #10029, #16300, #8212, #16413, #1733, #5000, #11629, #1835, #1619, #13322, #18106, #9714 ),
 ( #6706, #3526, #6815, #15019, #123, #14594, #13004, #8321, #19479, #11520, #6599, #221, #19893, #16512, #1927, #8423, #19793, #5215, #2037, #16616, #8532, #438, #6920, #13424, #16827, #4149, #12257, #2245, #7237, #3726, #8744, #2145, #8647, #13734, #20429, #964, #11829, #18735, #536, #15442, #5745, #3835, #18304, #11940, #753, #2350, #17033, #17140, #3936, #859, #2462, #10245, #16722, #13626, #8956, #7343, #7126, #20207, #5638, #2562, #10567, #15548, #20103, #7451, #15230, #12147, #15126, #643, #7017, #13516, #18626, #19992, #13948, #5421, #10677, #18417, #13835, #9059, #10357 ) ),
 .UNSPECIFIED., .F., .F., .F. ) 
 B_SPLINE_SURFACE_WITH_KNOTS ( ( 2, 2 ),
 ( 3, 2, 2, 2, 2, 2, 2, 2, 2, 2, 2, 2, 2, 2, 2, 2, 2, 2, 2, 2, 2, 2, 2, 2, 2, 2, 2, 2, 2, 2, 2, 2, 2, 2, 2, 2, 2, 2, 2, 3 ),
 ( 0.000000000000000000, 1.000000000000000000 ),
 ( 0.000000000000000000, 0.02500000000000000139, 0.05000000000000000278, 0.07499999999999999722, 0.1000000000000000056, 0.1250000000000000000, 0.1499999999999999944, 0.1749999999999999889, 0.2000000000000000111, 0.2250000000000000056, 0.2500000000000000000, 0.2750000000000000222, 0.2999999999999999889, 0.3250000000000000111, 0.3499999999999999778, 0.3750000000000000000, 0.4000000000000000222, 0.4249999999999999889, 0.4500000000000000111, 0.4749999999999999778, 0.5000000000000000000, 0.5250000000000000222, 0.5500000000000000444, 0.5749999999999999556, 0.5999999999999999778, 0.6250000000000000000, 0.6500000000000000222, 0.6750000000000000444, 0.6999999999999999556, 0.7249999999999999778, 0.7500000000000000000, 0.7750000000000000222, 0.8000000000000000444, 0.8249999999999999556, 0.8499999999999999778, 0.8750000000000000000, 0.9000000000000000222, 0.9250000000000000444, 0.9499999999999999556, 0.9600309957089442348 ),
 .UNSPECIFIED. ) 
 GEOMETRIC_REPRESENTATION_ITEM ( )  RATIONAL_B_SPLINE_SURFACE ( (
 ( 1.000000000000000000, 0.9238795325112867385, 1.000000000000000000, 0.9238795325112867385, 1.000000000000000000, 0.9238795325112867385, 1.000000000000000000, 0.9238795325112867385, 1.000000000000000000, 0.9238795325112867385, 1.000000000000000000, 0.9238795325112867385, 1.000000000000000000, 0.9238795325112867385, 1.000000000000000000, 0.9238795325112867385, 1.000000000000000000, 0.9238795325112867385, 1.000000000000000000, 0.9238795325112867385, 1.000000000000000000, 0.9238795325112867385, 1.000000000000000000, 0.9238795325112867385, 1.000000000000000000, 0.9238795325112867385, 1.000000000000000000, 0.9238795325112867385, 1.000000000000000000, 0.9238795325112867385, 1.000000000000000000, 0.9238795325112867385, 1.000000000000000000, 0.9238795325112867385, 1.000000000000000000, 0.9238795325112867385, 1.000000000000000000, 0.9238795325112867385, 1.000000000000000000, 0.9238795325112867385, 1.000000000000000000, 0.9238795325112867385, 1.000000000000000000, 0.9238795325112867385, 1.000000000000000000, 0.9238795325112867385, 1.000000000000000000, 0.9238795325112867385, 1.000000000000000000, 0.9238795325112867385, 1.000000000000000000, 0.9238795325112867385, 1.000000000000000000, 0.9238795325112867385, 1.000000000000000000, 0.9238795325112867385, 1.000000000000000000, 0.9238795325112867385, 1.000000000000000000, 0.9238795325112867385, 1.000000000000000000, 0.9238795325112867385, 1.000000000000000000, 0.9238795325112867385, 1.000000000000000000, 0.9238795325112867385, 1.000000000000000000, 0.9238795325112867385, 1.000000000000000000, 0.9238795325112867385, 1.000000000000000000, 0.9238795325112867385, 1.000000000000000000, 0.9238795325112867385, 1.000000000000000000, 0.9238795325112867385, 1.000000000000000000, 0.9694574366903154772, 0.9634246591005992677),
 ( 1.000000000000000000, 0.9238795325112867385, 1.000000000000000000, 0.9238795325112867385, 1.000000000000000000, 0.9238795325112867385, 1.000000000000000000, 0.9238795325112867385, 1.000000000000000000, 0.9238795325112867385, 1.000000000000000000, 0.9238795325112867385, 1.000000000000000000, 0.9238795325112867385, 1.000000000000000000, 0.9238795325112867385, 1.000000000000000000, 0.9238795325112867385, 1.000000000000000000, 0.9238795325112867385, 1.000000000000000000, 0.9238795325112867385, 1.000000000000000000, 0.9238795325112867385, 1.000000000000000000, 0.9238795325112867385, 1.000000000000000000, 0.9238795325112867385, 1.000000000000000000, 0.9238795325112867385, 1.000000000000000000, 0.9238795325112867385, 1.000000000000000000, 0.9238795325112867385, 1.000000000000000000, 0.9238795325112867385, 1.000000000000000000, 0.9238795325112867385, 1.000000000000000000, 0.9238795325112867385, 1.000000000000000000, 0.9238795325112867385, 1.000000000000000000, 0.9238795325112867385, 1.000000000000000000, 0.9238795325112867385, 1.000000000000000000, 0.9238795325112867385, 1.000000000000000000, 0.9238795325112867385, 1.000000000000000000, 0.9238795325112867385, 1.000000000000000000, 0.9238795325112867385, 1.000000000000000000, 0.9238795325112867385, 1.000000000000000000, 0.9238795325112867385, 1.000000000000000000, 0.9238795325112867385, 1.000000000000000000, 0.9238795325112867385, 1.000000000000000000, 0.9238795325112867385, 1.000000000000000000, 0.9238795325112867385, 1.000000000000000000, 0.9238795325112867385, 1.000000000000000000, 0.9238795325112867385, 1.000000000000000000, 0.9238795325112867385, 1.000000000000000000, 0.9238795325112867385, 1.000000000000000000, 0.9238795325112867385, 1.000000000000000000, 0.9694574366903154772, 0.9634246591005992677) ) ) 
 REPRESENTATION_ITEM ( '' )  SURFACE ( )  );
#2092 = DIRECTION ( 'NONE',  ( 1.000000000000000000, 0.000000000000000000, 0.000000000000000000 ) ) ;
#2093 = CARTESIAN_POINT ( 'NONE',  ( 6.154942347677927472, 50.94188193477284443, 75.39427037473855364 ) ) ;
#2095 = EDGE_CURVE ( 'NONE', #10737, #7917, #17515, .T. ) ;
#2094 = CARTESIAN_POINT ( 'NONE',  ( 5.579861850767188436, 50.61660611302658452, 76.99230741551831159 ) ) ;
#2096 = DIRECTION ( 'NONE',  ( -2.267473790562806355E-16, 5.922860397471811774E-17, -1.000000000000000000 ) ) ;
#2097 = ORIENTED_EDGE ( 'NONE', *, *, #1579, .T. ) ;
#2098 = EDGE_CURVE ( 'NONE', #4990, #3211, #9636, .T. ) ;
#2099 = ORIENTED_EDGE ( 'NONE', *, *, #13357, .T. ) ;
#2100 = CARTESIAN_POINT ( 'NONE',  ( 4.260580622453801425, 36.93752771366491316, 75.66510065906194882 ) ) ;
#2101 = CARTESIAN_POINT ( 'NONE',  ( 7.805461224862361824, 40.55160501283941699, 79.26294543469528264 ) ) ;
#2102 = ORIENTED_EDGE ( 'NONE', *, *, #8192, .F. ) ;
#2103 = VECTOR ( 'NONE', #7409, 1000.000000000000000 ) ;
#2104 = CARTESIAN_POINT ( 'NONE',  ( -4.909608826887576605, 38.01840769510402396, 75.43005142596166479 ) ) ;
#2105 = EDGE_CURVE ( 'NONE', #18429, #5501, #12826, .T. ) ;
#2106 = DIRECTION ( 'NONE',  ( 1.402518428993854849E-16, -1.000000000000000000, -1.734723475976787846E-14 ) ) ;
#2107 = CARTESIAN_POINT ( 'NONE',  ( -3.350035803220276609, 49.20851703305431357, 93.38308880123798872 ) ) ;
#2108 = AXIS2_PLACEMENT_3D ( 'NONE', #14350, #10864, #12443 ) ;
#2109 = VERTEX_POINT ( 'NONE', #6127 ) ;
#2110 = ADVANCED_FACE ( 'NONE', ( #20995 ), #11042, .T. ) ;
#2111 = DIRECTION ( 'NONE',  ( -1.193617070626243484E-16, -1.000000000000000000, 0.000000000000000000 ) ) ;
#2112 = VERTEX_POINT ( 'NONE', #1346 ) ;
#2113 = CARTESIAN_POINT ( 'NONE',  ( 2.263363662449363822, 49.77488197367694767, 93.19231768333818877 ) ) ;
#2114 = LINE ( 'NONE', #3692, #2259 ) ;
#2115 = CARTESIAN_POINT ( 'NONE',  ( -7.294472080575377326, 41.68420623513899415, 78.93669174070734584 ) ) ;
#2116 = LINE ( 'NONE', #5285, #18784 ) ;
#2117 = CARTESIAN_POINT ( 'NONE',  ( 11.22215374030649926, 39.96218137147969429, 80.55433879953099563 ) ) ;
#2118 = CARTESIAN_POINT ( 'NONE',  ( 8.272882475523552159, 41.50813378219739036, 75.97436175383765544 ) ) ;
#2120 = CARTESIAN_POINT ( 'NONE',  ( 27.03948732994508219, 27.61837231449496244, 73.00433879953101268 ) ) ;
#2119 = VECTOR ( 'NONE', #3701, 1000.000000000000000 ) ;
#2121 = DIRECTION ( 'NONE',  ( -1.196361017915039239E-16, 0.000000000000000000, 1.000000000000000000 ) ) ;
#2122 = CARTESIAN_POINT ( 'NONE',  ( 5.611423337425062385, 41.22389019960463230, 91.42996380123798872 ) ) ;
#2123 = CONICAL_SURFACE ( 'NONE', #6193, 4.000000000000003553, 0.7853981633974460586 ) ;
#2124 = LINE ( 'NONE', #12123, #12319 ) ;
#2125 = VERTEX_POINT ( 'NONE', #14320 ) ;
#2126 = CARTESIAN_POINT ( 'NONE',  ( 0.4078721606605034689, 52.35562703798189688, 76.01942718764288998 ) ) ;
#2127 = EDGE_LOOP ( 'NONE', ( #8859, #6030, #16934, #14120 ) ) ;
#2128 = CARTESIAN_POINT ( 'NONE',  ( 5.008975552073978932, 51.78836144432716537, 77.68963291717794561 ) ) ;
#2129 = ADVANCED_FACE ( 'NONE', ( #20894 ), #2733, .F. ) ;
#2130 = CARTESIAN_POINT ( 'NONE',  ( -4.534820675463383743, 37.71178600206382470, 78.55727908454632313 ) ) ;
#2131 = CARTESIAN_POINT ( 'NONE',  ( 4.394343283833276992, 39.11584570990505938, 92.75808880123797451 ) ) ;
#2132 = AXIS2_PLACEMENT_3D ( 'NONE', #16318, #5124, #37 ) ;
#2133 = CARTESIAN_POINT ( 'NONE',  ( -7.154059339130676598, 47.04588606493869918, 72.45433879953087342 ) ) ;
#2134 = CARTESIAN_POINT ( 'NONE',  ( 7.753636062665578699, 48.02814353133176439, 72.45433879953087342 ) ) ;
#2135 = CARTESIAN_POINT ( 'NONE',  ( 5.509674309642067058, 50.66539996488663178, 78.02050120841747116 ) ) ;
#2136 = ORIENTED_EDGE ( 'NONE', *, *, #3471, .F. ) ;
#2137 = ORIENTED_EDGE ( 'NONE', *, *, #15661, .T. ) ;
#2138 = CARTESIAN_POINT ( 'NONE',  ( 8.412752068583754905, 42.37169419728517994, 79.44701590970058191 ) ) ;
#2139 = LINE ( 'NONE', #12141, #4304 ) ;
#2140 = CARTESIAN_POINT ( 'NONE',  ( 5.544276951911416340, 50.64433212932689088, 78.27786821129558348 ) ) ;
#2141 = ORIENTED_EDGE ( 'NONE', *, *, #6732, .T. ) ;
#2142 = CARTESIAN_POINT ( 'NONE',  ( 0.8450648237196969337, 52.96353724031100541, 78.65078808693101564 ) ) ;
#2143 = CARTESIAN_POINT ( 'NONE',  ( -2.389205813017604374, 39.09668198135606332, 95.05433879953093879 ) ) ;
#2144 = CARTESIAN_POINT ( 'NONE',  ( 4.199109002476567376, 47.83913663364971569, 95.05036078555451695 ) ) ;
#2145 = CARTESIAN_POINT ( 'NONE',  ( -0.2125050281363792815, 38.58189400963055959, 93.30496380294501080 ) ) ;
#2146 = CARTESIAN_POINT ( 'NONE',  ( 24.43948732994508788, 43.16218137147969003, 74.70433879953100131 ) ) ;
#2147 = VECTOR ( 'NONE', #1642, 1000.000000000000000 ) ;
#2148 = B_SPLINE_CURVE_WITH_KNOTS ( 'NONE', 3,
 ( #19060, #17658, #3094, #9595, #12566, #2885, #8091, #11299, #2982, #4468, #4881 ),
 .UNSPECIFIED., .F., .F.,
 ( 4, 1, 1, 1, 1, 1, 1, 1, 4 ),
 ( 0.000000000000000000, 0.1208544691022559597, 0.2402546218586821825, 0.3598696579477268509, 0.4809300011950208842, 0.6037041574249993880, 0.7308714335393303729, 0.8631644367168944676, 0.9999999999999998890 ),
 .UNSPECIFIED. ) ;
#2149 = CARTESIAN_POINT ( 'NONE',  ( 5.611423337425062385, 41.22389019960463230, 93.92996380123798872 ) ) ;
#2150 = UNCERTAINTY_MEASURE_WITH_UNIT (LENGTH_MEASURE( 1.000000000000000082E-05 ), #2681, 'distance_accuracy_value', 'NONE');
#2151 = CARTESIAN_POINT ( 'NONE',  ( 4.432284427945813121, 36.14044538431356557, 77.43080938776617472 ) ) ;
#2152 = ORIENTED_EDGE ( 'NONE', *, *, #1461, .T. ) ;
#2153 = LINE ( 'NONE', #8652, #16368 ) ;
#2154 = ORIENTED_EDGE ( 'NONE', *, *, #16533, .F. ) ;
#2155 = CARTESIAN_POINT ( 'NONE',  ( -1.219056181836355446, 49.77488197367695477, 93.15612966814926210 ) ) ;
#2156 = CARTESIAN_POINT ( 'NONE',  ( -2.077846259693550746, 39.65884927180063357, 95.72683880294496817 ) ) ;
#2157 = VERTEX_POINT ( 'NONE', #2811 ) ;
#2158 = CARTESIAN_POINT ( 'NONE',  ( 6.722153740306509917, 44.16218137147969003, 80.55433879953099563 ) ) ;
#2159 = VECTOR ( 'NONE', #4458, 1000.000000000000000 ) ;
#2160 = CARTESIAN_POINT ( 'NONE',  ( -1.477846259693498254, 49.81903562097207327, 59.21119304902337888 ) ) ;
#2161 = CARTESIAN_POINT ( 'NONE',  ( 8.787829143201870252, 41.13140593384865440, 77.80727997600146750 ) ) ;
#2162 = DIRECTION ( 'NONE',  ( -0.7071067811865535679, 1.203855704449247279E-16, -0.7071067811865414665 ) ) ;
#2163 = CARTESIAN_POINT ( 'NONE',  ( 31.22215374030650281, 42.96218137147968008, 77.40433879953098995 ) ) ;
#2164 = VERTEX_POINT ( 'NONE', #19281 ) ;
#2165 = CARTESIAN_POINT ( 'NONE',  ( 2.522153740306510628, 47.62628298661744708, 53.15433879953100416 ) ) ;
#2166 = EDGE_CURVE ( 'NONE', #122, #3564, #20766, .T. ) ;
#2167 = ORIENTED_EDGE ( 'NONE', *, *, #8591, .T. ) ;
#2168 = CARTESIAN_POINT ( 'NONE',  ( -3.677846259693500652, 44.16218137147969003, 54.55433879953099563 ) ) ;
#2169 = CARTESIAN_POINT ( 'NONE',  ( -6.932661394073498684, 41.01730649666358630, 77.07900976289242578 ) ) ;
#2170 = CARTESIAN_POINT ( 'NONE',  ( 5.568489401881125289, 48.03437091500647682, 93.07058880123797451 ) ) ;
#2171 = CARTESIAN_POINT ( 'NONE',  ( 5.430500802020164386, 37.59341706865419042, 76.00983965925686903 ) ) ;
#2172 = CARTESIAN_POINT ( 'NONE',  ( -3.628867371436362621, 48.69222599884265179, 91.23558879782397923 ) ) ;
#2173 = EDGE_CURVE ( 'NONE', #279, #18072, #8618, .T. ) ;
#2174 = AXIS2_PLACEMENT_3D ( 'NONE', #4794, #3000, #1622 ) ;
#2175 = VERTEX_POINT ( 'NONE', #20570 ) ;
#2176 = CARTESIAN_POINT ( 'NONE',  ( 11.22215374030650281, 42.96218137147968008, 61.40715055817103263 ) ) ;
#2177 = ORIENTED_EDGE ( 'NONE', *, *, #126, .F. ) ;
#2178 = PLANE ( 'NONE',  #2728 ) ;
#2179 = CARTESIAN_POINT ( 'NONE',  ( -2.077846259693550746, 39.65884927180063357, 92.91433879953098085 ) ) ;
#2180 = CARTESIAN_POINT ( 'NONE',  ( -3.981178359372548492, 46.76218137147973408, 95.10183879953099506 ) ) ;
#2181 = ORIENTED_EDGE ( 'NONE', *, *, #4678, .F. ) ;
#2182 = CARTESIAN_POINT ( 'NONE',  ( -4.209923912819722780, 38.70632820095286775, 77.90139762306027649 ) ) ;
#2183 = DIRECTION ( 'NONE',  ( 1.290716872006552287E-16, 1.000000000000000000, 0.000000000000000000 ) ) ;
#2184 = VERTEX_POINT ( 'NONE', #5997 ) ;
#2186 = CARTESIAN_POINT ( 'NONE',  ( 5.750640099535992533, 51.24052371918730842, 75.36022115247205022 ) ) ;
#2185 = B_SPLINE_CURVE_WITH_KNOTS ( 'NONE', 3,
 ( #5206, #3303, #12996, #16294, #213, #1829, #16503, #17987, #3616, #3412, #14792, #9922, #3519, #10023, #1920, #5738, #7231, #2344, #854, #10672, #4034, #12248, #17135, #13729, #18730, #8735, #11823 ),
 .UNSPECIFIED., .F., .F.,
 ( 4, 1, 1, 1, 1, 1, 1, 1, 1, 1, 1, 1, 1, 1, 1, 1, 1, 1, 1, 1, 1, 1, 1, 1, 4 ),
 ( 0.000000000000000000, 0.04981064803454772483, 0.09714544705284619552, 0.1414600528990057893, 0.1834992459999073566, 0.2227657660311612720, 0.2600403684493295953, 0.2949019026928859644, 0.3281718573768891978, 0.3602550803352915776, 0.3926260793274650163, 0.4253773651182169435, 0.4592860034499685606, 0.4939555262694102500, 0.5299277977440765008, 0.5677681756169172811, 0.6073809588441169138, 0.6486765994917140787, 0.6919144726687150859, 0.7374495574558619371, 0.7851062196494249523, 0.8349986418379958808, 0.8875444209637680659, 0.9425288195084158271, 1.000000000000000000 ),
 .UNSPECIFIED. ) ;
#2187 = DIRECTION ( 'NONE',  ( 1.110223024625156294E-16, -1.000000000000000000, -7.183611964723542594E-17 ) ) ;
#2188 = VERTEX_POINT ( 'NONE', #4389 ) ;
#2189 = CARTESIAN_POINT ( 'NONE',  ( 1.997688547473374099, 52.22837930658135264, 78.99477371038418028 ) ) ;
#2190 = ORIENTED_EDGE ( 'NONE', *, *, #19409, .F. ) ;
#2191 = CARTESIAN_POINT ( 'NONE',  ( 0.7971746217111946864, 52.35757360625640189, 77.48431181218198560 ) ) ;
#2192 = LINE ( 'NONE', #13998, #673 ) ;
#2193 = CARTESIAN_POINT ( 'NONE',  ( 4.394343283833276992, 39.11584570990505938, 91.35183880123798872 ) ) ;
#2194 = CARTESIAN_POINT ( 'NONE',  ( -3.533185125431080653, 36.21728222759318072, 78.38559710128819802 ) ) ;
#2195 = CARTESIAN_POINT ( 'NONE',  ( -5.661408436751226070, 39.74363423441516829, 72.45433879953085921 ) ) ;
#2196 = CARTESIAN_POINT ( 'NONE',  ( 6.450247442662826458, 38.49669771550791353, 76.69330938776616335 ) ) ;
#2197 = EDGE_CURVE ( 'NONE', #4469, #16470, #10915, .T. ) ;
#2198 = VERTEX_POINT ( 'NONE', #12601 ) ;
#2199 = CARTESIAN_POINT ( 'NONE',  ( 5.722153740306500147, 44.16218137147968292, 93.33161078214054385 ) ) ;
#2200 = VERTEX_POINT ( 'NONE', #15900 ) ;
#2201 = CARTESIAN_POINT ( 'NONE',  ( 8.787829143201870252, 41.13140593384865440, 77.80727997600146750 ) ) ;
#2202 = DIRECTION ( 'NONE',  ( -4.731737692062721725E-17, 0.7071067811865525687, 0.7071067811865425767 ) ) ;
#2203 = CARTESIAN_POINT ( 'NONE',  ( 5.568489401881125289, 48.03437091500646261, 94.32058880123798872 ) ) ;
#2204 = CARTESIAN_POINT ( 'NONE',  ( -3.496280357775573222, 52.10652770678432688, 75.88277413867518817 ) ) ;
#2205 = ORIENTED_EDGE ( 'NONE', *, *, #15377, .F. ) ;
#2206 = CARTESIAN_POINT ( 'NONE',  ( 6.921466148593897749, 50.37568168049836714, 78.61296362383696135 ) ) ;
#2207 = ORIENTED_EDGE ( 'NONE', *, *, #15920, .T. ) ;
#2208 = DIRECTION ( 'NONE',  ( 0.3165065846431930341, 0.9485903129789495791, 2.188653791613884362E-16 ) ) ;
#2209 = ADVANCED_FACE ( 'NONE', ( #9412 ), #16002, .F. ) ;
#2210 = CARTESIAN_POINT ( 'NONE',  ( 5.701723800661059549, 37.96731586519243251, 75.40772603260481333 ) ) ;
#2211 = EDGE_CURVE ( 'NONE', #18929, #2282, #6718, .T. ) ;
#2212 = PLANE ( 'NONE',  #17884 ) ;
#2214 = EDGE_CURVE ( 'NONE', #14909, #13986, #7781, .T. ) ;
#2213 = CARTESIAN_POINT ( 'NONE',  ( 4.097638513832391638, 51.53669645659447696, 76.64209438045911327 ) ) ;
#2215 = LINE ( 'NONE', #4973, #5167 ) ;
#2216 = LINE ( 'NONE', #10751, #7952 ) ;
#2217 = CARTESIAN_POINT ( 'NONE',  ( 0.6017860623987091317, 52.35409786639082341, 77.38437845781280089 ) ) ;
#2218 = CARTESIAN_POINT ( 'NONE',  ( 1.443767556222832260, 38.34550624821717690, 92.55433879953092458 ) ) ;
#2219 = CARTESIAN_POINT ( 'NONE',  ( -4.517072128342570991, 36.94403992325788977, 76.81463291717793140 ) ) ;
#2220 = EDGE_CURVE ( 'NONE', #1879, #18554, #5121, .T. ) ;
#2221 = CARTESIAN_POINT ( 'NONE',  ( 4.394343283833276992, 39.11584570990505938, 93.85183880123797451 ) ) ;
#2222 = EDGE_CURVE ( 'NONE', #11233, #557, #8432, .T. ) ;
#2223 = CARTESIAN_POINT ( 'NONE',  ( -1.123656915330052408, 35.37488560990637865, 76.86610350541323555 ) ) ;
#2224 = ORIENTED_EDGE ( 'NONE', *, *, #6602, .T. ) ;
#2225 = LINE ( 'NONE', #3916, #12943 ) ;
#2226 = ORIENTED_EDGE ( 'NONE', *, *, #9928, .F. ) ;
#2227 = CARTESIAN_POINT ( 'NONE',  ( 5.216235101676203634, 50.88570979358116375, 77.12281451049645398 ) ) ;
#2228 = CARTESIAN_POINT ( 'NONE',  ( 1.514255888186003984, 52.36218137147968577, 83.03825919817350609 ) ) ;
#2229 = CARTESIAN_POINT ( 'NONE',  ( -3.349688636638950889, 52.21127678364309332, 78.10580938776615767 ) ) ;
#2230 = CARTESIAN_POINT ( 'NONE',  ( 5.611423337425062385, 41.22389019960463230, 95.33621380123798872 ) ) ;
#2231 = CARTESIAN_POINT ( 'NONE',  ( -4.895412223390202655, 37.22350451100091817, 76.36316342150684022 ) ) ;
#2232 = DIRECTION ( 'NONE',  ( 1.000000000000000000, -1.110223024625156540E-16, 1.779391786395883043E-16 ) ) ;
#2233 = CARTESIAN_POINT ( 'NONE',  ( 1.352400422481993658, 50.46853102219002096, 91.97683880123797451 ) ) ;
#2234 = CARTESIAN_POINT ( 'NONE',  ( -1.477846259693498920, 47.62628298661744708, 66.55433879953099563 ) ) ;
#2235 = ORIENTED_EDGE ( 'NONE', *, *, #6169, .T. ) ;
#2236 = EDGE_LOOP ( 'NONE', ( #1193, #16651, #19748, #1602, #7326 ) ) ;
#2237 = B_SPLINE_CURVE_WITH_KNOTS ( 'NONE', 3,
 ( #2509, #15387, #18352, #694, #7174, #9002, #15489, #17492, #13990, #18983, #12404, #18884, #9417, #9629, #11225, #1007, #1427, #10819, #4598, #16007, #14092, #12605, #17590, #14295, #19092, #7609, #12498 ),
 .UNSPECIFIED., .F., .F.,
 ( 4, 1, 1, 1, 1, 1, 1, 1, 1, 1, 1, 1, 1, 1, 1, 1, 1, 1, 1, 1, 1, 1, 1, 1, 4 ),
 ( 0.000000000000000000, 0.04992685941337848821, 0.09871136507264777205, 0.1457954968408328167, 0.1915776562037285746, 0.2364429891513756543, 0.2798905081306632403, 0.3226114784840122263, 0.3640369619956516645, 0.4040931382756795531, 0.4423864865660626644, 0.4791244981183566676, 0.5145420102664520767, 0.5484747442263178119, 0.5814193454185596632, 0.6141157465626525536, 0.6462545211269067336, 0.6795390940691592441, 0.7156628256359011120, 0.7545220547839790459, 0.7966562418723396322, 0.8423152836035615598, 0.8912945236129800053, 0.9437207944264596193, 1.000000000000000000 ),
 .UNSPECIFIED. ) ;
#2238 = CARTESIAN_POINT ( 'NONE',  ( 9.201390675156970289, 42.37087608097247227, 79.34093170394821470 ) ) ;
#2239 = CARTESIAN_POINT ( 'NONE',  ( 8.787829143201870252, 41.13140593384865440, 77.14698585835439815 ) ) ;
#2240 = CARTESIAN_POINT ( 'NONE',  ( 0.5221537403065188432, 44.16218137147969003, 54.55433879953099563 ) ) ;
#2241 = ORIENTED_EDGE ( 'NONE', *, *, #12352, .T. ) ;
#2242 = CARTESIAN_POINT ( 'NONE',  ( -1.477846259693502473, 47.62628298661744708, 74.55433879953100984 ) ) ;
#2243 = CARTESIAN_POINT ( 'NONE',  ( -4.927956858767000625, 44.38046240684710142, 95.05433879953103826 ) ) ;
#2244 = CARTESIAN_POINT ( 'NONE',  ( 0.5221537403065015237, 49.16218137147969003, 92.72886871425484401 ) ) ;
#2245 = CARTESIAN_POINT ( 'NONE',  ( 6.102441102155617969, 43.42752260303680600, 93.61746380294498238 ) ) ;
#2246 = EDGE_CURVE ( 'NONE', #4602, #14794, #3429, .T. ) ;
#2247 = CARTESIAN_POINT ( 'NONE',  ( -7.199075288064514133, 41.41206959199826088, 78.61536821129558916 ) ) ;
#2248 = CARTESIAN_POINT ( 'NONE',  ( 2.043125170982144745, 38.48583871533720213, 95.02371380123798872 ) ) ;
#2249 = PRODUCT_DEFINITION_SHAPE ( 'NONE', 'NONE',  #21042 ) ;
#2250 = CARTESIAN_POINT ( 'NONE',  ( 10.77494014480653561, 42.76218137147968434, 69.80574467885101342 ) ) ;
#2251 = VERTEX_POINT ( 'NONE', #9941 ) ;
#2252 = LINE ( 'NONE', #19696, #1761 ) ;
#2253 = ORIENTED_EDGE ( 'NONE', *, *, #20354, .T. ) ;
#2254 = CARTESIAN_POINT ( 'NONE',  ( -4.477846259693498254, 50.66218137147966871, 53.35433879953099989 ) ) ;
#2255 = CARTESIAN_POINT ( 'NONE',  ( 3.122153740306552905, 48.66551347115873227, 95.10183880294498238 ) ) ;
#2256 = ORIENTED_EDGE ( 'NONE', *, *, #534, .F. ) ;
#2257 = CARTESIAN_POINT ( 'NONE',  ( -4.283496025856503131, 47.84326572019833179, 72.45433879953087342 ) ) ;
#2258 = CARTESIAN_POINT ( 'NONE',  ( -3.467962453771612275, 40.50591351489411096, 94.75121379953098710 ) ) ;
#2259 = VECTOR ( 'NONE', #20180, 1000.000000000000000 ) ;
#2260 = CARTESIAN_POINT ( 'NONE',  ( -3.926839636664805511, 51.79886580987140832, 79.42193487995672285 ) ) ;
#2261 = CARTESIAN_POINT ( 'NONE',  ( 4.393996117251955269, 36.11308595931626542, 76.96022115247204454 ) ) ;
#2262 = DIRECTION ( 'NONE',  ( -1.000000000000000000, 0.000000000000000000, 0.000000000000000000 ) ) ;
#2263 = DIRECTION ( 'NONE',  ( -1.779391786395883536E-16, -5.922860397471806844E-17, 1.000000000000000000 ) ) ;
#2264 = ORIENTED_EDGE ( 'NONE', *, *, #11861, .F. ) ;
#2265 = DIRECTION ( 'NONE',  ( 1.193617070626243237E-16, 1.000000000000000000, 1.876284981264363171E-30 ) ) ;
#2266 = VERTEX_POINT ( 'NONE', #10041 ) ;
#2267 = DIRECTION ( 'NONE',  ( 1.779391786395883536E-16, 5.922860397471806844E-17, -1.000000000000000000 ) ) ;
#2268 = CARTESIAN_POINT ( 'NONE',  ( 2.122153740306496505, 50.16218137147969713, 69.55433879953100984 ) ) ;
#2269 = CARTESIAN_POINT ( 'NONE',  ( 5.309255083855641821, 37.50457964663987553, 75.97198585835440099 ) ) ;
#2270 = CARTESIAN_POINT ( 'NONE',  ( -5.616286711741429905, 44.43019146960381960, 92.64183879782400766 ) ) ;
#2271 = CARTESIAN_POINT ( 'NONE',  ( 6.573693162767834330, 44.00881163587200717, 75.45433879953087342 ) ) ;
#2272 = VECTOR ( 'NONE', #7583, 1000.000000000000000 ) ;
#2273 = CARTESIAN_POINT ( 'NONE',  ( -4.387981331227590154, 51.46935083841186298, 75.37146543928014353 ) ) ;
#2274 = ORIENTED_EDGE ( 'NONE', *, *, #13438, .F. ) ;
#2275 = DIRECTION ( 'NONE',  ( 0.000000000000000000, 0.000000000000000000, -1.000000000000000000 ) ) ;
#2276 = ADVANCED_FACE ( 'NONE', ( #1745 ), #8225, .T. ) ;
#2277 = ORIENTED_EDGE ( 'NONE', *, *, #16165, .F. ) ;
#2278 = DIRECTION ( 'NONE',  ( -1.000000000000000000, 1.193617070626243237E-16, -5.626130192357177659E-16 ) ) ;
#2279 = CARTESIAN_POINT ( 'NONE',  ( -4.500660556396669065, 42.81632233694663370, 95.25808879953098085 ) ) ;
#2280 = CARTESIAN_POINT ( 'NONE',  ( -0.8237052942265477018, 49.18499566818285018, 92.44558879953099506 ) ) ;
#2281 = CARTESIAN_POINT ( 'NONE',  ( -8.007168758255900798, 41.92872724082349123, 77.34580771017452605 ) ) ;
#2282 = VERTEX_POINT ( 'NONE', #16315 ) ;
#2283 = FACE_OUTER_BOUND ( 'NONE', #12410, .T. ) ;
#2284 = CARTESIAN_POINT ( 'NONE',  ( 30.92220646078100188, 42.76218137147968434, 62.80715055817104542 ) ) ;
#2285 = LINE ( 'NONE', #17083, #16612 ) ;
#2286 = LINE ( 'NONE', #7389, #16302 ) ;
#2287 = CARTESIAN_POINT ( 'NONE',  ( 3.122153740306552905, 48.66551347115873227, 92.28933879953099506 ) ) ;
#2288 = VERTEX_POINT ( 'NONE', #14711 ) ;
#2289 = CARTESIAN_POINT ( 'NONE',  ( -7.609845089999874190, 43.10833364818387992, 76.06610350541322418 ) ) ;
#2290 = CARTESIAN_POINT ( 'NONE',  ( -0.3080929418689875576, 37.85583172076933778, 93.85183880123797451 ) ) ;
#2291 = AXIS2_PLACEMENT_3D ( 'NONE', #11494, #13290, #6360 ) ;
#2292 = ORIENTED_EDGE ( 'NONE', *, *, #2813, .T. ) ;
#2293 = CARTESIAN_POINT ( 'NONE',  ( -4.804644443005473775, 51.17161863374556674, 76.44036821129557779 ) ) ;
#2294 = CARTESIAN_POINT ( 'NONE',  ( 0.5221537403065010796, 44.16218137147969003, 45.55433879953098852 ) ) ;
#2295 = CARTESIAN_POINT ( 'NONE',  ( -2.416137431568557314, 39.07291177436112406, 91.11746380123798872 ) ) ;
#2296 = CONTEXT_DEPENDENT_SHAPE_REPRESENTATION ( #6266, #24 ) ;
#2297 = CARTESIAN_POINT ( 'NONE',  ( -0.4699484075730042676, 52.36218137147968577, 52.53721119516358584 ) ) ;
#2298 = AXIS2_PLACEMENT_3D ( 'NONE', #15629, #17708, #4819 ) ;
#2299 = CARTESIAN_POINT ( 'NONE',  ( 0.5221537403065077410, 49.16218137147969003, 94.29136871766880290 ) ) ;
#2300 = ORIENTED_EDGE ( 'NONE', *, *, #14790, .T. ) ;
#2301 = ORIENTED_EDGE ( 'NONE', *, *, #10196, .F. ) ;
#2302 = EDGE_CURVE ( 'NONE', #10971, #16740, #14912, .T. ) ;
#2303 = CARTESIAN_POINT ( 'NONE',  ( 2.002180786195896900, 52.20240726524163932, 75.93722239247614425 ) ) ;
#2304 = VECTOR ( 'NONE', #18591, 1000.000000000000000 ) ;
#2305 = VERTEX_POINT ( 'NONE', #337 ) ;
#2306 = FACE_BOUND ( 'NONE', #1922, .T. ) ;
#2307 = CARTESIAN_POINT ( 'NONE',  ( 0.3594029150778950688, 52.35600914658472504, 77.51213090161979835 ) ) ;
#2308 = CARTESIAN_POINT ( 'NONE',  ( -5.784195910403845176, 44.99242805365518194, 96.03933880123796030 ) ) ;
#2309 = ORIENTED_EDGE ( 'NONE', *, *, #1184, .T. ) ;
#2310 = LINE ( 'NONE', #10421, #15056 ) ;
#2311 = ORIENTED_EDGE ( 'NONE', *, *, #4534, .F. ) ;
#2312 = CARTESIAN_POINT ( 'NONE',  ( 2.522153740306507075, 50.16218137147969713, 74.55433879953100984 ) ) ;
#2313 = DIRECTION ( 'NONE',  ( 1.084202172485505420E-16, 1.000000000000000000, 0.000000000000000000 ) ) ;
#2314 = CIRCLE ( 'NONE', #8775, 4.000000000000003553 ) ;
#2315 = ADVANCED_FACE ( 'NONE', ( #16426 ), #5301, .T. ) ;
#2316 = DIRECTION ( 'NONE',  ( 1.402518428993831183E-16, -1.000000000000000000, 3.469446951953617640E-16 ) ) ;
#2317 = CARTESIAN_POINT ( 'NONE',  ( -7.375807652561674033, 41.95680328822960092, 78.70894555753855570 ) ) ;
#2318 = DIRECTION ( 'NONE',  ( 0.6546536707079709805, 0.6546536707079818607, -0.3779644730092299176 ) ) ;
#2319 = CARTESIAN_POINT ( 'NONE',  ( -5.154188915835984375, 42.64120994080404614, 94.86746380123797451 ) ) ;
#2320 = CARTESIAN_POINT ( 'NONE',  ( 0.7603968142568129363, 52.96420094791147903, 77.43909148762901395 ) ) ;
#2321 = FACE_OUTER_BOUND ( 'NONE', #11770, .T. ) ;
#2322 = CARTESIAN_POINT ( 'NONE',  ( 5.089266475819410829, 50.80422082628552261, 75.36789977960694387 ) ) ;
#2323 = CARTESIAN_POINT ( 'NONE',  ( -0.2125050281363792815, 38.58189400963055959, 94.55496380294496817 ) ) ;
#2324 = DIRECTION ( 'NONE',  ( -0.3855022007253699479, 0.1286266402413967502, -0.9136975652020240535 ) ) ;
#2325 = ORIENTED_EDGE ( 'NONE', *, *, #15698, .F. ) ;
#2326 =( LENGTH_UNIT ( ) NAMED_UNIT ( * ) SI_UNIT ( .MILLI., .METRE. ) );
#2327 = APPLICATION_CONTEXT ( 'automotive_design' ) ;
#2328 = EDGE_CURVE ( 'NONE', #9181, #8749, #7593, .T. ) ;
#2329 = EDGE_CURVE ( 'NONE', #6705, #502, #19256, .T. ) ;
#2330 = AXIS2_PLACEMENT_3D ( 'NONE', #11746, #18220, #16431 ) ;
#2331 = ORIENTED_EDGE ( 'NONE', *, *, #8190, .F. ) ;
#2332 = CARTESIAN_POINT ( 'NONE',  ( 30.92220646078100188, 42.76218137147968434, 56.80715055817104542 ) ) ;
#2333 = PLANE ( 'NONE',  #7182 ) ;
#2334 = CARTESIAN_POINT ( 'NONE',  ( 2.263811127080452845, 49.90383875825364157, 77.41268141275706682 ) ) ;
#2335 = CARTESIAN_POINT ( 'NONE',  ( -3.350035803220276609, 49.20851703305431357, 93.38308880123798872 ) ) ;
#2336 = CARTESIAN_POINT ( 'NONE',  ( -4.517072128342570991, 36.94403992325788977, 76.81463291717793140 ) ) ;
#2337 = DIRECTION ( 'NONE',  ( -0.3165065846431826535, -0.9485903129789527988, 0.000000000000000000 ) ) ;
#2338 = CARTESIAN_POINT ( 'NONE',  ( -1.477846259693499364, 47.62628298661744708, 69.15433879953098995 ) ) ;
#2339 = EDGE_CURVE ( 'NONE', #19914, #10724, #11510, .T. ) ;
#2340 = CARTESIAN_POINT ( 'NONE',  ( 3.948530577815479337, 39.69684013992245752, 93.46121380294498238 ) ) ;
#2341 = EDGE_LOOP ( 'NONE', ( #11895, #5818, #19485, #17485, #7605, #7895 ) ) ;
#2342 = VERTEX_POINT ( 'NONE', #8093 ) ;
#2343 = CARTESIAN_POINT ( 'NONE',  ( 9.263154249150899133, 42.55598543044034443, 79.20437336408532758 ) ) ;
#2344 = CARTESIAN_POINT ( 'NONE',  ( -4.002011967609276688, 36.56358573041305249, 75.49480657079904233 ) ) ;
#2345 = DIRECTION ( 'NONE',  ( 1.193617070626243237E-16, 1.000000000000000000, 1.898669798061574161E-30 ) ) ;
#2346 = CARTESIAN_POINT ( 'NONE',  ( 5.799728954038464224, 51.20426375978601641, 77.28794373216803137 ) ) ;
#2347 = LINE ( 'NONE', #20727, #1620 ) ;
#2348 = VECTOR ( 'NONE', #11097, 1000.000000000000227 ) ;
#2349 = CARTESIAN_POINT ( 'NONE',  ( -8.190409139795066906, 42.92474528817020740, 76.06610350541322418 ) ) ;
#2350 = CARTESIAN_POINT ( 'NONE',  ( 3.948530577815480225, 39.69684013992245752, 92.21121380294495395 ) ) ;
#2351 = CARTESIAN_POINT ( 'NONE',  ( -0.2933318293205740002, 52.92496007935942259, 79.40378080832554986 ) ) ;
#2352 = CARTESIAN_POINT ( 'NONE',  ( -7.701322689919003039, 47.31527676703458951, 78.22140724958771330 ) ) ;
#2353 = CARTESIAN_POINT ( 'NONE',  ( -2.416137431568557314, 39.07291177436112406, 93.61746380123797451 ) ) ;
#2354 = CARTESIAN_POINT ( 'NONE',  ( 6.774925554820337759, 37.81441096401221102, 75.87985893138584004 ) ) ;
#2355 = ORIENTED_EDGE ( 'NONE', *, *, #4557, .F. ) ;
#2356 = EDGE_CURVE ( 'NONE', #5798, #4528, #1487, .T. ) ;
#2357 = CARTESIAN_POINT ( 'NONE',  ( 1.309422257521039024, 52.32623752027490127, 75.43140154991867519 ) ) ;
#2358 = VECTOR ( 'NONE', #13013, 1000.000000000000000 ) ;
#2359 = ORIENTED_EDGE ( 'NONE', *, *, #16564, .F. ) ;
#2360 = DIRECTION ( 'NONE',  ( -0.000000000000000000, -2.168404344970984413E-15, -1.000000000000000000 ) ) ;
#2361 = ADVANCED_FACE ( 'NONE', ( #16082 ), #13094, .T. ) ;
#2362 = CARTESIAN_POINT ( 'NONE',  ( 5.544968037009670780, 45.50804040601273925, 94.94558880294498238 ) ) ;
#2363 = EDGE_LOOP ( 'NONE', ( #12852, #210, #5950, #18962 ) ) ;
#2364 = CARTESIAN_POINT ( 'NONE',  ( 5.856396280011940014, 46.10368687828906076, 93.34496379782399345 ) ) ;
#2365 = EDGE_CURVE ( 'NONE', #16412, #20669, #5266, .T. ) ;
#2367 = CIRCLE ( 'NONE', #662, 3.999999999999996447 ) ;
#2366 = DIRECTION ( 'NONE',  ( -9.598494438985367424E-18, 5.922860397471809309E-17, -1.000000000000000000 ) ) ;
#2368 = CARTESIAN_POINT ( 'NONE',  ( -3.425442721482995445, 52.15714568814760810, 78.86270620133520026 ) ) ;
#2369 = DIRECTION ( 'NONE',  ( -1.000000000000000000, 0.000000000000000000, -0.000000000000000000 ) ) ;
#2370 = CARTESIAN_POINT ( 'NONE',  ( 0.8505931169942170245, 52.96356605174086951, 76.42615000023204175 ) ) ;
#2371 = CARTESIAN_POINT ( 'NONE',  ( 0.5672115121316617659, 52.96572379054431678, 78.93584868477675798 ) ) ;
#2372 = ORIENTED_EDGE ( 'NONE', *, *, #7430, .T. ) ;
#2373 = CARTESIAN_POINT ( 'NONE',  ( -7.617292153972126556, 43.16748516956134551, 72.45433879953085921 ) ) ;
#2374 = VECTOR ( 'NONE', #12084, 1000.000000000000114 ) ;
#2375 = ORIENTED_EDGE ( 'NONE', *, *, #17785, .T. ) ;
#2376 = DIRECTION ( 'NONE',  ( -1.110223024625156540E-16, -1.000000000000000000, -5.922860397471808077E-17 ) ) ;
#2377 = CARTESIAN_POINT ( 'NONE',  ( -3.099028042286850138, 36.80507306568591019, 78.38160280800818214 ) ) ;
#2378 = DIRECTION ( 'NONE',  ( -0.3165065846431826535, -0.9485903129789527988, 0.000000000000000000 ) ) ;
#2379 = VECTOR ( 'NONE', #13162, 1000.000000000000000 ) ;
#2380 = VECTOR ( 'NONE', #19902, 1000.000000000000114 ) ;
#2381 = CARTESIAN_POINT ( 'NONE',  ( 6.467578312573260213, 50.71095034124950729, 79.40187404227555135 ) ) ;
#2382 = DIRECTION ( 'NONE',  ( -0.9996789974703352843, 0.02533578529877050789, -1.494306935163143217E-16 ) ) ;
#2383 = CARTESIAN_POINT ( 'NONE',  ( -4.812088799398939187, 42.22067586467031930, 92.71996379782397923 ) ) ;
#2384 = CARTESIAN_POINT ( 'NONE',  ( -5.251100579623896536, 37.48623717174979220, 75.42164981362142839 ) ) ;
#2385 = VECTOR ( 'NONE', #7392, 1000.000000000000000 ) ;
#2386 = VERTEX_POINT ( 'NONE', #3005 ) ;
#2387 = CARTESIAN_POINT ( 'NONE',  ( 8.865792162213244509, 41.36506604770743678, 78.93669174070734584 ) ) ;
#2388 = ORIENTED_EDGE ( 'NONE', *, *, #14063, .F. ) ;
#2389 = CARTESIAN_POINT ( 'NONE',  ( 30.92220646078100188, 42.96218137147968008, 58.20715055817105110 ) ) ;
#2390 = EDGE_CURVE ( 'NONE', #10307, #1377, #14391, .T. ) ;
#2391 = CARTESIAN_POINT ( 'NONE',  ( -3.981178359372548492, 46.76218137147973408, 95.10183879953099506 ) ) ;
#2392 = CARTESIAN_POINT ( 'NONE',  ( -3.981178359372548492, 46.76218137147973408, 91.35183879953098085 ) ) ;
#2393 = ORIENTED_EDGE ( 'NONE', *, *, #2596, .T. ) ;
#2394 = AXIS2_PLACEMENT_3D ( 'NONE', #17774, #1394, #9289 ) ;
#2395 = CARTESIAN_POINT ( 'NONE',  ( -4.567115856812060670, 47.10047254335474065, 94.71121380123797451 ) ) ;
#2396 = CARTESIAN_POINT ( 'NONE',  ( 0.5472186751089482826, 52.96225730869564075, 77.38586825451125151 ) ) ;
#2397 = ORIENTED_EDGE ( 'NONE', *, *, #3532, .T. ) ;
#2398 = CARTESIAN_POINT ( 'NONE',  ( 1.851481395807867303, 48.14626068599128672, 79.40903933791013003 ) ) ;
#2399 = LINE ( 'NONE', #801, #20706 ) ;
#2400 = EDGE_LOOP ( 'NONE', ( #7586, #711, #14166, #3451 ) ) ;
#2401 = CARTESIAN_POINT ( 'NONE',  ( 2.021724605155154286, 52.22392082761901122, 78.95144739612317153 ) ) ;
#2402 = CARTESIAN_POINT ( 'NONE',  ( 6.198496396448986090, 45.68315280215533392, 95.49246380123798872 ) ) ;
#2403 = VECTOR ( 'NONE', #9178, 1000.000000000000000 ) ;
#2404 = ORIENTED_EDGE ( 'NONE', *, *, #14317, .T. ) ;
#2405 = CARTESIAN_POINT ( 'NONE',  ( 0.8448918989077306430, 52.35582772558348097, 77.71799948569541527 ) ) ;
#2406 = CARTESIAN_POINT ( 'NONE',  ( 25.03948732994508219, 43.16218137147969003, 74.70433879953100131 ) ) ;
#2407 = PRODUCT_CONTEXT ( 'NONE', #11728, 'mechanical' ) ;
#2408 = CARTESIAN_POINT ( 'NONE',  ( -7.677846259693478892, 49.36218137147968577, 93.55433879953098142 ) ) ;
#2409 = PRODUCT_DEFINITION_FORMATION_WITH_SPECIFIED_SOURCE ( 'ANY', '', #3765, .NOT_KNOWN. ) ;
#2410 = CARTESIAN_POINT ( 'NONE',  ( 0.5886017282102210535, 52.96193049659134999, 78.93669174070734584 ) ) ;
#2411 = B_SPLINE_CURVE_WITH_KNOTS ( 'NONE', 3,
 ( #12264, #18531, #17356, #20541, #5870, #13742, #17247, #1085, #5548, #8861, #2357, #20212, #12463, #2671, #20322, #9175 ),
 .UNSPECIFIED., .F., .F.,
 ( 4, 2, 2, 2, 2, 2, 2, 4 ),
 ( 0.000000000000000000, 0.0002719588327788573625, 0.0005439176655577147249, 0.0008158764983365720874, 0.001087835331115429450, 0.001631752996673123575, 0.001903711829451970854, 0.002175670662230817700 ),
 .UNSPECIFIED. ) ;
#2412 = CARTESIAN_POINT ( 'NONE',  ( 5.241460166982749413, 50.86801069014953924, 72.45433879953087342 ) ) ;
#2413 = EDGE_CURVE ( 'NONE', #9137, #15270, #302, .T. ) ;
#2414 = ORIENTED_EDGE ( 'NONE', *, *, #13793, .F. ) ;
#2415 = ORIENTED_EDGE ( 'NONE', *, *, #16270, .T. ) ;
#2416 = CARTESIAN_POINT ( 'NONE',  ( 1.383856401949368875, 52.20728298024938141, 75.46169036918907125 ) ) ;
#2417 = ORIENTED_EDGE ( 'NONE', *, *, #16993, .T. ) ;
#2418 = FACE_OUTER_BOUND ( 'NONE', #18268, .T. ) ;
#2419 = FACE_OUTER_BOUND ( 'NONE', #3614, .T. ) ;
#2420 = CARTESIAN_POINT ( 'NONE',  ( -3.350035803220276609, 49.20851703305431357, 94.63308880123798872 ) ) ;
#2421 = ORIENTED_EDGE ( 'NONE', *, *, #10000, .F. ) ;
#2422 = VERTEX_POINT ( 'NONE', #11012 ) ;
#2423 = CARTESIAN_POINT ( 'NONE',  ( 6.467578312573260213, 50.71095034124950729, 79.40187404227555135 ) ) ;
#2424 = VECTOR ( 'NONE', #5350, 1000.000000000000000 ) ;
#2425 = ORIENTED_EDGE ( 'NONE', *, *, #12252, .T. ) ;
#2426 = LINE ( 'NONE', #4111, #13508 ) ;
#2427 = DIRECTION ( 'NONE',  ( -1.540237394707284220E-16, -1.793354297423764243E-16, 1.000000000000000000 ) ) ;
#2428 = PLANE ( 'NONE',  #15528 ) ;
#2429 = CARTESIAN_POINT ( 'NONE',  ( -4.142301312995646079, 50.90705069304581087, 79.54681934798814780 ) ) ;
#2430 = CARTESIAN_POINT ( 'NONE',  ( -7.594845318933780121, 42.99712684704532961, 78.99675904272704940 ) ) ;
#2431 = CARTESIAN_POINT ( 'NONE',  ( 6.198496396448986090, 45.68315280215533392, 95.49246380123798872 ) ) ;
#2432 = B_SPLINE_SURFACE_WITH_KNOTS ( 'NONE', 3, 1, ( 
 ( #14715, #14815 ),
 ( #6721, #18219 ),
 ( #13227, #13335 ),
 ( #19704, #10045 ),
 ( #16524, #1944 ),
 ( #14915, #340 ),
 ( #5229, #16630 ),
 ( #2051, #11797 ),
 ( #3691, #15093 ),
 ( #13485, #19956 ),
 ( #5387, #3802 ),
 ( #15193, #18492 ),
 ( #10426, #16893 ),
 ( #20179, #5609 ),
 ( #14119, #4113 ),
 ( #20501, #7638 ),
 ( #19123, #20394 ),
 ( #4322, #2847 ),
 ( #4221, #5933 ),
 ( #18810, #4536 ),
 ( #10747, #13909 ),
 ( #9029, #12430 ),
 ( #10849, #7314 ),
 ( #15836, #17209 ),
 ( #9350, #2634 ),
 ( #1247, #10643 ),
 ( #9135, #7416 ),
 ( #7740, #17110 ),
 ( #15622, #5824 ),
 ( #1044, #7530 ),
 ( #4437, #6029 ) ),
 .UNSPECIFIED., .F., .F., .F.,
 ( 4, 1, 1, 1, 1, 1, 1, 1, 1, 1, 1, 1, 1, 1, 1, 1, 1, 1, 1, 1, 1, 1, 1, 1, 1, 1, 1, 1, 4 ),
 ( 2, 2 ),
 ( 0.000000000000000000, 0.04402879139878041609, 0.08604540006880039005, 0.1260521755942069777, 0.1641511405281330660, 0.2003442918647115323, 0.2347805632357193584, 0.2676267374383518027, 0.2986515534027265328, 0.3283031585252670914, 0.3570062744687346745, 0.3846398569069188755, 0.4113091075058319390, 0.4372322170293685417, 0.4625237182236557887, 0.4872935253130181721, 0.5115235732650775802, 0.5580727247437320404, 0.6018864549903041317, 0.6437727082467282758, 0.6848253805047307408, 0.7076001045990409910, 0.7352252901417971609, 0.7674583008524621386, 0.8043075748156178761, 0.8460289209228792906, 0.8926357087385640154, 0.9438729761760307202, 1.000000000000000000 ),
 ( 0.000000000000000000, 1.000000000000000000 ),
 .UNSPECIFIED. ) ;
#2433 = CARTESIAN_POINT ( 'NONE',  ( 0.8452388978709587386, 52.35217815131273511, 77.74134350746754762 ) ) ;
#2434 = EDGE_CURVE ( 'NONE', #1854, #17442, #641, .T. ) ;
#2435 = CARTESIAN_POINT ( 'NONE',  ( 2.522153740306511516, 50.16218137147969713, 50.55433879953100273 ) ) ;
#2436 = PLANE ( 'NONE',  #12586 ) ;
#2437 = CARTESIAN_POINT ( 'NONE',  ( 1.256812508749381774, 49.74246873332880625, 91.42996380294499659 ) ) ;
#2438 = AXIS2_PLACEMENT_3D ( 'NONE', #6668, #19647, #16682 ) ;
#2439 = CARTESIAN_POINT ( 'NONE',  ( -7.955859814585196865, 41.77362178188068498, 78.62287654527649750 ) ) ;
#2440 =( NAMED_UNIT ( * ) PLANE_ANGLE_UNIT ( ) SI_UNIT ( $, .RADIAN. ) );
#2441 = VECTOR ( 'NONE', #10969, 1000.000000000000000 ) ;
#2442 = VERTEX_POINT ( 'NONE', #12793 ) ;
#2443 = CARTESIAN_POINT ( 'NONE',  ( 5.184346195548571679, 46.85389944066466228, 94.99612681657399094 ) ) ;
#2444 = ADVANCED_FACE ( 'NONE', ( #1416 ), #17690, .T. ) ;
#2445 = CARTESIAN_POINT ( 'NONE',  ( 5.750640099535992533, 51.24052371918730842, 75.36022115247205022 ) ) ;
#2446 = DIRECTION ( 'NONE',  ( -4.731737692062685363E-17, 0.7071067811865536790, 0.7071067811865414665 ) ) ;
#2447 = CARTESIAN_POINT ( 'NONE',  ( -4.524181921268124462, 40.28999182795290324, 94.94558880123797451 ) ) ;
#2448 = CARTESIAN_POINT ( 'NONE',  ( -5.135517778528630117, 37.40086081253994621, 77.33633635728615729 ) ) ;
#2449 = CARTESIAN_POINT ( 'NONE',  ( -7.607193028824243086, 43.12151120863332920, 78.28007409364852265 ) ) ;
#2450 = CARTESIAN_POINT ( 'NONE',  ( 5.564133502460520297, 36.94922329332227662, 77.75193993234761081 ) ) ;
#2451 = CARTESIAN_POINT ( 'NONE',  ( -3.943187491250720544, 40.73580453397070755, 93.14871380294496817 ) ) ;
#2452 = ORIENTED_EDGE ( 'NONE', *, *, #324, .T. ) ;
#2453 = ORIENTED_EDGE ( 'NONE', *, *, #630, .F. ) ;
#2454 = VECTOR ( 'NONE', #7597, 1000.000000000000000 ) ;
#2455 = CARTESIAN_POINT ( 'NONE',  ( 6.519648887156654915, 49.75415655210358068, 76.85154547133247149 ) ) ;
#2456 = CARTESIAN_POINT ( 'NONE',  ( -5.667418469993653396, 43.80274312437727247, 80.45433879953087342 ) ) ;
#2457 = CARTESIAN_POINT ( 'NONE',  ( 8.951667845840693971, 41.62244091939069790, 76.38301527011910252 ) ) ;
#2458 = AXIS2_PLACEMENT_3D ( 'NONE', #18855, #4062, #14162 ) ;
#2459 = CARTESIAN_POINT ( 'NONE',  ( 5.936990147225109204, 51.10287444559717329, 77.01219674908871582 ) ) ;
#2460 = PLANE ( 'NONE',  #17589 ) ;
#2461 = CARTESIAN_POINT ( 'NONE',  ( 9.080605399405701661, 42.00887494707089331, 78.12791555553386047 ) ) ;
#2462 = CARTESIAN_POINT ( 'NONE',  ( -4.500660556396669065, 42.81632233694663370, 91.82058880294496817 ) ) ;
#2463 = B_SPLINE_CURVE_WITH_KNOTS ( 'NONE', 3,
 ( #13365, #18150, #9976, #16457, #6956, #14846, #1877, #19934, #3569, #10075, #8469, #14952, #373, #6858 ),
 .UNSPECIFIED., .F., .F.,
 ( 4, 2, 2, 2, 2, 2, 4 ),
 ( 0.000000000000000000, 0.0001566759795594400181, 0.0003133519591188800362, 0.0003916899488986000724, 0.0004700279386783201086, 0.0005483659284580401447, 0.0006267039182377599641 ),
 .UNSPECIFIED. ) ;
#2464 = DIRECTION ( 'NONE',  ( -1.193617070626243484E-16, -1.000000000000000000, -0.000000000000000000 ) ) ;
#2465 = CARTESIAN_POINT ( 'NONE',  ( -6.879319821983923333, 47.65235040223281260, 78.32456649736994336 ) ) ;
#2466 = CARTESIAN_POINT ( 'NONE',  ( -5.154188915835984375, 42.64120994080404614, 92.21121380123797451 ) ) ;
#2467 = VECTOR ( 'NONE', #6966, 1000.000000000000114 ) ;
#2468 = EDGE_CURVE ( 'NONE', #16604, #12459, #6783, .T. ) ;
#2469 = CARTESIAN_POINT ( 'NONE',  ( -7.912665105161496903, 41.65176285775086029, 79.54689059276779517 ) ) ;
#2470 = CARTESIAN_POINT ( 'NONE',  ( 5.853612939038055352, 51.16446183064613251, 78.89719962956496602 ) ) ;
#2471 = VECTOR ( 'NONE', #6575, 1000.000000000000000 ) ;
#2472 = FACE_OUTER_BOUND ( 'NONE', #3003, .T. ) ;
#2473 = ORIENTED_EDGE ( 'NONE', *, *, #8472, .F. ) ;
#2474 = CARTESIAN_POINT ( 'NONE',  ( -4.766891056059167298, 51.19859582181767621, 78.86176377286571437 ) ) ;
#2475 = CARTESIAN_POINT ( 'NONE',  ( 5.611423337425062385, 41.22389019960463230, 92.67996380123798872 ) ) ;
#2476 = ORIENTED_EDGE ( 'NONE', *, *, #17478, .T. ) ;
#2477 = DIRECTION ( 'NONE',  ( 1.779391786395883536E-16, 5.922860397471805611E-17, -1.000000000000000000 ) ) ;
#2478 = CARTESIAN_POINT ( 'NONE',  ( -0.5863195729081822627, 39.16218137147969003, 94.87115272619178086 ) ) ;
#2479 = CARTESIAN_POINT ( 'NONE',  ( -3.387980870927748800, 52.18391455498849751, 78.68920376838389075 ) ) ;
#2480 = CARTESIAN_POINT ( 'NONE',  ( 0.5915428171209280439, 52.96190779654647685, 77.38375056423674891 ) ) ;
#2481 = FACE_OUTER_BOUND ( 'NONE', #5850, .T. ) ;
#2482 = LINE ( 'NONE', #8977, #8934 ) ;
#2483 = ORIENTED_EDGE ( 'NONE', *, *, #3782, .T. ) ;
#2484 = ADVANCED_FACE ( 'NONE', ( #20656 ), #14493, .T. ) ;
#2485 = CARTESIAN_POINT ( 'NONE',  ( 5.360476111768327279, 50.78276677175456655, 77.95007283232945383 ) ) ;
#2486 = VECTOR ( 'NONE', #10396, 1000.000000000000000 ) ;
#2487 = ORIENTED_EDGE ( 'NONE', *, *, #11341, .T. ) ;
#2488 = CARTESIAN_POINT ( 'NONE',  ( 6.485595322925789219, 49.79047067704939877, 78.31989234064305094 ) ) ;
#2489 = CARTESIAN_POINT ( 'NONE',  ( 4.546108750497564799, 52.13026250523957827, 76.88467537290178200 ) ) ;
#2490 = ADVANCED_FACE ( 'NONE', ( #7599 ), #9406, .T. ) ;
#2491 = CARTESIAN_POINT ( 'NONE',  ( 0.3201111382462868971, 51.36399839264385037, 76.44919174070734869 ) ) ;
#2492 = CARTESIAN_POINT ( 'NONE',  ( -7.437180633310755518, 40.40796476851179619, 77.62507288737846523 ) ) ;
#2493 = DIRECTION ( 'NONE',  ( 1.000000000000000000, 0.000000000000000000, 0.000000000000000000 ) ) ;
#2494 = CARTESIAN_POINT ( 'NONE',  ( 5.807735516834878986, 37.12329237395520920, 76.04105433551922033 ) ) ;
#2495 = CARTESIAN_POINT ( 'NONE',  ( -5.623541984526490012, 37.76134463469641389, 75.60525969576029581 ) ) ;
#2496 = EDGE_CURVE ( 'NONE', #16100, #15360, #19007, .T. ) ;
#2497 = EDGE_CURVE ( 'NONE', #9206, #17046, #455, .T. ) ;
#2498 = ORIENTED_EDGE ( 'NONE', *, *, #7498, .F. ) ;
#2499 = CARTESIAN_POINT ( 'NONE',  ( 8.211482387076870282, 41.32431627734197832, 78.55826321071354812 ) ) ;
#2500 = ORIENTED_EDGE ( 'NONE', *, *, #7029, .F. ) ;
#2501 = AXIS2_PLACEMENT_3D ( 'NONE', #13027, #4916, #16013 ) ;
#2502 = CARTESIAN_POINT ( 'NONE',  ( -4.126251043470592350, 50.73659813720719569, 75.36123162944792853 ) ) ;
#2503 = CARTESIAN_POINT ( 'NONE',  ( 4.987494971863720927, 47.58855820898865829, 95.96121379953099506 ) ) ;
#2504 = ORIENTED_EDGE ( 'NONE', *, *, #19447, .T. ) ;
#2505 = CARTESIAN_POINT ( 'NONE',  ( -0.3080929418689875576, 37.85583172076933778, 93.85183880123797451 ) ) ;
#2506 = CARTESIAN_POINT ( 'NONE',  ( -4.007890887056452023, 40.01116025973682611, 95.14183879782397923 ) ) ;
#2507 = CARTESIAN_POINT ( 'NONE',  ( 5.561379608955574483, 51.38032281970146897, 76.39036821129558064 ) ) ;
#2508 = EDGE_LOOP ( 'NONE', ( #18283, #15086, #7600, #17745 ) ) ;
#2509 = CARTESIAN_POINT ( 'NONE',  ( 5.665287683258889651, 37.02150436742986273, 75.36022115247205022 ) ) ;
#2510 = CARTESIAN_POINT ( 'NONE',  ( -3.677846259693500652, 44.16218137147969003, 45.55433879953098852 ) ) ;
#2511 = VERTEX_POINT ( 'NONE', #15211 ) ;
#2512 = CARTESIAN_POINT ( 'NONE',  ( 2.722153740306518799, 44.16218137147969003, 54.55433879953099563 ) ) ;
#2513 = VERTEX_POINT ( 'NONE', #13405 ) ;
#2514 = CARTESIAN_POINT ( 'NONE',  ( -5.405939962049822967, 49.82766502745145232, 78.10580938776615767 ) ) ;
#2515 = DIRECTION ( 'NONE',  ( -0.3165065846431827090, -0.9485903129789527988, 0.000000000000000000 ) ) ;
#2516 = AXIS2_PLACEMENT_3D ( 'NONE', #11801, #14774, #18277 ) ;
#2517 = PRODUCT_CONTEXT ( 'NONE', #19720, 'mechanical' ) ;
#2518 = DIRECTION ( 'NONE',  ( 0.5813877811927011807, -0.8136266022444372803, -5.636455622144619183E-17 ) ) ;
#2519 = EDGE_CURVE ( 'NONE', #11891, #7289, #17983, .T. ) ;
#2520 = CARTESIAN_POINT ( 'NONE',  ( 5.393087686338805753, 50.75151780712509009, 78.93669174070734584 ) ) ;
#2521 = CARTESIAN_POINT ( 'NONE',  ( 11.22215374030650281, 45.56218137147968861, 78.80433879953099563 ) ) ;
#2522 = ORIENTED_EDGE ( 'NONE', *, *, #1302, .F. ) ;
#2523 = CARTESIAN_POINT ( 'NONE',  ( -6.850209527372854268, 47.75220363455441230, 78.32492703482499508 ) ) ;
#2524 = ORIENTED_EDGE ( 'NONE', *, *, #17073, .T. ) ;
#2525 = CARTESIAN_POINT ( 'NONE',  ( 29.63948732994508006, 45.16218137147968292, 74.70433879953100131 ) ) ;
#2526 = LINE ( 'NONE', #921, #2103 ) ;
#2527 = CARTESIAN_POINT ( 'NONE',  ( -3.350035803220276609, 49.20851703305431357, 92.13308880123798872 ) ) ;
#2528 = CARTESIAN_POINT ( 'NONE',  ( -3.373440834332912086, 52.19430433279444514, 76.25796290525131838 ) ) ;
#2529 = ORIENTED_EDGE ( 'NONE', *, *, #16507, .F. ) ;
#2530 = CARTESIAN_POINT ( 'NONE',  ( -7.333990156426536622, 40.19720935722482125, 75.45433879953087342 ) ) ;
#2531 = ORIENTED_EDGE ( 'NONE', *, *, #6063, .T. ) ;
#2532 = CARTESIAN_POINT ( 'NONE',  ( 4.468221962074742315, 51.27377933314817682, 79.33697856897433098 ) ) ;
#2533 = CARTESIAN_POINT ( 'NONE',  ( -1.677846259693499542, 47.73989013547934945, 50.15433879953098995 ) ) ;
#2534 = LINE ( 'NONE', #14221, #20125 ) ;
#2535 = CARTESIAN_POINT ( 'NONE',  ( -4.645483384943265293, 37.03889214578788369, 77.94562699264550076 ) ) ;
#2536 = CARTESIAN_POINT ( 'NONE',  ( -7.068211413017330358, 41.44596913834843122, 79.53187240040659844 ) ) ;
#2537 = CARTESIAN_POINT ( 'NONE',  ( 6.882736312352589536, 37.89144858414100270, 77.26022115247205591 ) ) ;
#2538 = FACE_OUTER_BOUND ( 'NONE', #6775, .T. ) ;
#2539 = CARTESIAN_POINT ( 'NONE',  ( -4.848575437813097189, 50.22045157099402957, 75.48294376282896678 ) ) ;
#2540 =( NAMED_UNIT ( * ) PLANE_ANGLE_UNIT ( ) SI_UNIT ( $, .RADIAN. ) );
#2541 = CARTESIAN_POINT ( 'NONE',  ( 3.948530577815480225, 39.69684013992245752, 93.46121380294496817 ) ) ;
#2542 = CARTESIAN_POINT ( 'NONE',  ( 1.215246153217547587, 50.28109722957945849, 83.67325465763077830 ) ) ;
#2543 = EDGE_LOOP ( 'NONE', ( #20116, #7012, #11650, #5179 ) ) ;
#2544 = CARTESIAN_POINT ( 'NONE',  ( 8.295230459923363497, 41.57513201800704650, 78.93627637315103129 ) ) ;
#2545 = ORIENTED_EDGE ( 'NONE', *, *, #1954, .T. ) ;
#2546 = DIRECTION ( 'NONE',  ( -0.3165065846431829311, -0.9485903129789527988, -2.188653791613874255E-16 ) ) ;
#2547 = LINE ( 'NONE', #5623, #20082 ) ;
#2548 = CARTESIAN_POINT ( 'NONE',  ( -4.370691255933373931, 51.48170569318705247, 79.53937015691786883 ) ) ;
#2549 = CARTESIAN_POINT ( 'NONE',  ( -4.453436368711327198, 50.68011839687689957, 76.44036821129557779 ) ) ;
#2550 = EDGE_CURVE ( 'NONE', #19372, #10780, #8827, .T. ) ;
#2551 = CARTESIAN_POINT ( 'NONE',  ( -4.842431058766297980, 37.18436945890474021, 76.00936707281648808 ) ) ;
#2552 = CARTESIAN_POINT ( 'NONE',  ( -7.498699170063192199, 42.77841955502557170, 79.26478910100486530 ) ) ;
#2553 = CARTESIAN_POINT ( 'NONE',  ( 8.480805917192030918, 42.18208851247151614, 78.13498589288056451 ) ) ;
#2554 = CARTESIAN_POINT ( 'NONE',  ( -4.338703338798237219, 37.56692202555748139, 75.97299512023676016 ) ) ;
#2555 = ORIENTED_EDGE ( 'NONE', *, *, #15105, .T. ) ;
#2556 = CARTESIAN_POINT ( 'NONE',  ( 8.214799251806553571, 41.32260305165857517, 78.45948585835439815 ) ) ;
#2557 = CARTESIAN_POINT ( 'NONE',  ( 0.5221537403065010796, 44.16218137147968292, 78.25433879953088478 ) ) ;
#2558 = CARTESIAN_POINT ( 'NONE',  ( 8.945167944750011202, 41.60296030347588214, 76.15680935856015310 ) ) ;
#2559 = CARTESIAN_POINT ( 'NONE',  ( -5.955451856753747109, 38.00651308716548726, 77.05433879953086773 ) ) ;
#2560 = DIRECTION ( 'NONE',  ( 2.838338907332122006E-16, -1.000000000000000000, 0.000000000000000000 ) ) ;
#2561 = CARTESIAN_POINT ( 'NONE',  ( -4.101343092926645895, 50.93446548159070630, 78.88986109003506897 ) ) ;
#2562 = CARTESIAN_POINT ( 'NONE',  ( 6.102441102155617969, 43.42752260303680600, 91.11746380294498238 ) ) ;
#2563 = CARTESIAN_POINT ( 'NONE',  ( -4.536263512923754959, 51.36339382032895884, 75.97373057797423712 ) ) ;
#2564 = CARTESIAN_POINT ( 'NONE',  ( -7.517776057030331138, 47.86537766978320718, 78.32456649736994336 ) ) ;
#2565 = CARTESIAN_POINT ( 'NONE',  ( -5.492848774261456235, 38.60081332101042051, 78.80728580974474085 ) ) ;
#2566 = CARTESIAN_POINT ( 'NONE',  ( 5.991756872021341884, 37.25478729691962343, 75.38041148603002739 ) ) ;
#2567 = ORIENTED_EDGE ( 'NONE', *, *, #17772, .T. ) ;
#2568 = CARTESIAN_POINT ( 'NONE',  ( 5.799728954038464224, 51.20426375978601641, 77.28794373216803137 ) ) ;
#2569 = ORIENTED_EDGE ( 'NONE', *, *, #3990, .F. ) ;
#2570 = EDGE_CURVE ( 'NONE', #11438, #5268, #734, .T. ) ;
#2571 = DIRECTION ( 'NONE',  ( 1.540237394707283727E-16, 1.793354297423763257E-16, -1.000000000000000000 ) ) ;
#2572 = CARTESIAN_POINT ( 'NONE',  ( -2.904223097202481174, 48.62752260303690122, 91.58621380294496817 ) ) ;
#2573 = ORIENTED_EDGE ( 'NONE', *, *, #20426, .F. ) ;
#2574 = CARTESIAN_POINT ( 'NONE',  ( 6.522560395309022319, 49.75102024682771429, 76.63889762306028786 ) ) ;
#2575 = CARTESIAN_POINT ( 'NONE',  ( 5.025485839985549319, 41.56218137147963887, 94.47683879953099506 ) ) ;
#2576 = CARTESIAN_POINT ( 'NONE',  ( -4.007802336140563249, 51.74101282905964894, 79.45569801420249689 ) ) ;
#2577 = LINE ( 'NONE', #15564, #3997 ) ;
#2578 = CARTESIAN_POINT ( 'NONE',  ( 5.755371611800503828, 51.23702874167446453, 77.28963291717792572 ) ) ;
#2579 = CYLINDRICAL_SURFACE ( 'NONE', #18092, 6.000000000000001776 ) ;
#2580 = VERTEX_POINT ( 'NONE', #2332 ) ;
#2581 = CARTESIAN_POINT ( 'NONE',  ( 5.599231707071657738, 51.35236299959863970, 78.59183879953087626 ) ) ;
#2582 = CARTESIAN_POINT ( 'NONE',  ( 2.463659247115867146, 38.82793883177424732, 92.87621379782399345 ) ) ;
#2583 = EDGE_CURVE ( 'NONE', #10346, #4844, #12893, .T. ) ;
#2584 = ORIENTED_EDGE ( 'NONE', *, *, #16663, .T. ) ;
#2585 = DIRECTION ( 'NONE',  ( 1.193617070626243484E-16, 1.000000000000000000, 0.000000000000000000 ) ) ;
#2586 = DIRECTION ( 'NONE',  ( -0.3164955768080224829, -0.9485573217986537076, 0.008340091313796951095 ) ) ;
#2587 = CARTESIAN_POINT ( 'NONE',  ( 2.043125170982144745, 38.48583871533720213, 92.67996380123798872 ) ) ;
#2588 = CARTESIAN_POINT ( 'NONE',  ( 8.214799251806553571, 41.32260305165857517, 76.40801527011910821 ) ) ;
#2589 = EDGE_CURVE ( 'NONE', #14804, #7531, #685, .T. ) ;
#2590 = DIRECTION ( 'NONE',  ( -1.000000000000000000, 0.000000000000000000, -1.196361017915039239E-16 ) ) ;
#2591 = CARTESIAN_POINT ( 'NONE',  ( 5.658108625003792191, 37.01637447524286273, 75.97198585835440099 ) ) ;
#2592 = DIRECTION ( 'NONE',  ( -0.9485903129789527988, 0.3165065846431829311, -8.934458285744989980E-17 ) ) ;
#2593 = ORIENTED_EDGE ( 'NONE', *, *, #10000, .T. ) ;
#2594 = CARTESIAN_POINT ( 'NONE',  ( -1.117719678584871090, 36.12782917792895176, 76.86610350541323555 ) ) ;
#2595 = EDGE_CURVE ( 'NONE', #18174, #2513, #3369, .T. ) ;
#2596 = EDGE_CURVE ( 'NONE', #14483, #4403, #5297, .T. ) ;
#2597 = ADVANCED_FACE ( 'NONE', ( #16596 ), #10443, .T. ) ;
#2598 = EDGE_LOOP ( 'NONE', ( #13106, #7378, #18979, #1998 ) ) ;
#2599 = CIRCLE ( 'NONE', #18221, 4.200000000000003730 ) ;
#2600 = CARTESIAN_POINT ( 'NONE',  ( -4.561334846378493069, 51.34547876336230843, 75.36123162944792853 ) ) ;
#2601 = CARTESIAN_POINT ( 'NONE',  ( 4.394343283833276992, 39.11584570990505938, 95.25808880123800293 ) ) ;
#2602 = ORIENTED_EDGE ( 'NONE', *, *, #19010, .T. ) ;
#2603 = CARTESIAN_POINT ( 'NONE',  ( 6.198496396448986090, 45.68315280215533392, 91.74246380123798872 ) ) ;
#2604 = LINE ( 'NONE', #12187, #12335 ) ;
#2605 = CARTESIAN_POINT ( 'NONE',  ( 2.273808892390292602, 39.34717618618597612, 95.05433879953095300 ) ) ;
#2606 = CARTESIAN_POINT ( 'NONE',  ( -4.804644443005473775, 51.17161863374555963, 78.45066232894264147 ) ) ;
#2607 = EDGE_CURVE ( 'NONE', #11628, #26, #8722, .T. ) ;
#2608 = VERTEX_POINT ( 'NONE', #20084 ) ;
#2609 = CARTESIAN_POINT ( 'NONE',  ( 2.114739078132396255, 52.20604064652322762, 78.26567215968707103 ) ) ;
#2610 = CARTESIAN_POINT ( 'NONE',  ( -5.784195910403845176, 44.99242805365518194, 92.28933880123798872 ) ) ;
#2611 = ORIENTED_EDGE ( 'NONE', *, *, #14253, .T. ) ;
#2612 = CARTESIAN_POINT ( 'NONE',  ( -5.357560295633086334, 49.87790279705807706, 78.82253136475043220 ) ) ;
#2613 = CARTESIAN_POINT ( 'NONE',  ( 5.098362185591304829, 37.35789059091872133, 76.18266185049213846 ) ) ;
#2614 = APPLICATION_CONTEXT ( 'automotive_design' ) ;
#2615 = AXIS2_PLACEMENT_3D ( 'NONE', #3207, #8205, #8098 ) ;
#2616 = SHAPE_DEFINITION_REPRESENTATION ( #20075, #9739 ) ;
#2617 = CARTESIAN_POINT ( 'NONE',  ( 5.089995120079088942, 37.35733679680688368, 76.23948081211554495 ) ) ;
#2618 = CARTESIAN_POINT ( 'NONE',  ( 5.497686461428984650, 36.90174267058258550, 76.03636210503219672 ) ) ;
#2619 = LINE ( 'NONE', #2521, #10976 ) ;
#2620 = EDGE_LOOP ( 'NONE', ( #20047, #13665, #8384, #10803, #9095, #3104, #13366, #8279, #8531, #17090, #3209, #16887, #13096, #6702, #13259, #9211, #3516, #10318, #9607, #15390, #89, #10911, #8733, #3179, #20477, #13924, #7805, #20552, #18372, #10236 ) ) ;
#2621 = CARTESIAN_POINT ( 'NONE',  ( 1.086229506649126764, 52.96246798893113805, 75.39315892328370694 ) ) ;
#2622 = EDGE_LOOP ( 'NONE', ( #13279, #1805, #3995, #7696 ) ) ;
#2623 = CARTESIAN_POINT ( 'NONE',  ( 6.532049803590284753, 50.66332784790530752, 75.53514883118299394 ) ) ;
#2624 = EDGE_CURVE ( 'NONE', #16845, #682, #5521, .T. ) ;
#2625 = PLANE ( 'NONE',  #18408 ) ;
#2626 = CARTESIAN_POINT ( 'NONE',  ( -4.567115856812060670, 47.10047254335474065, 95.80496380123798872 ) ) ;
#2627 = ORIENTED_EDGE ( 'NONE', *, *, #13685, .T. ) ;
#2628 = AXIS2_PLACEMENT_3D ( 'NONE', #7555, #14043, #5952 ) ;
#2629 = EDGE_CURVE ( 'NONE', #17396, #13246, #16906, .T. ) ;
#2630 = CARTESIAN_POINT ( 'NONE',  ( -3.246606053099431843, 48.47200184337508233, 92.45433879953098710 ) ) ;
#2631 = VERTEX_POINT ( 'NONE', #15110 ) ;
#2632 = CARTESIAN_POINT ( 'NONE',  ( 5.455102971993217587, 51.45882509034149166, 79.53290755650829169 ) ) ;
#2633 = LINE ( 'NONE', #5823, #4713 ) ;
#2634 = CARTESIAN_POINT ( 'NONE',  ( 7.674368124774328948, 40.17547738449357553, 76.47636794762235013 ) ) ;
#2635 = EDGE_CURVE ( 'NONE', #2902, #4298, #5758, .T. ) ;
#2636 = ORIENTED_EDGE ( 'NONE', *, *, #12225, .T. ) ;
#2637 = CARTESIAN_POINT ( 'NONE',  ( -4.753731435370070812, 37.11885062014071934, 77.91594000873737969 ) ) ;
#2638 = CARTESIAN_POINT ( 'NONE',  ( 5.894623494294806143, 51.13416898548390321, 78.12411320240556734 ) ) ;
#2639 = CARTESIAN_POINT ( 'NONE',  ( -4.477846259693498254, 50.66218137147966871, 53.35433879953099989 ) ) ;
#2640 = CARTESIAN_POINT ( 'NONE',  ( 1.658154530501163793, 36.04125148601230677, 75.45433879953087342 ) ) ;
#2641 = LINE ( 'NONE', #7644, #9458 ) ;
#2642 = VECTOR ( 'NONE', #7234, 1000.000000000000000 ) ;
#2643 = CARTESIAN_POINT ( 'NONE',  ( 0.7004076996470288696, 52.96039943697842745, 78.90962015830227472 ) ) ;
#2644 = DIRECTION ( 'NONE',  ( -0.2741027427660463478, -0.8215033088236058934, -0.4999999999999977240 ) ) ;
#2645 = EDGE_CURVE ( 'NONE', #12080, #3841, #20018, .T. ) ;
#2646 = CARTESIAN_POINT ( 'NONE',  ( -3.943187491250720544, 40.73580453397070755, 94.39871380294496817 ) ) ;
#2647 = VECTOR ( 'NONE', #17448, 1000.000000000000114 ) ;
#2648 = CARTESIAN_POINT ( 'NONE',  ( -7.465935398647475907, 40.46964184340244230, 79.25534888921224308 ) ) ;
#2649 = DIRECTION ( 'NONE',  ( 0.5813877811925719508, -0.8136266022445296509, 1.938039666723524832E-13 ) ) ;
#2650 =( BOUNDED_CURVE ( )  B_SPLINE_CURVE ( 3, ( #2334, #20298, #2653, #15427 ),
 .UNSPECIFIED., .F., .F. ) 
 B_SPLINE_CURVE_WITH_KNOTS ( ( 4, 4 ),
 ( 5.006904465492824308, 5.052225889838808826 ),
 .UNSPECIFIED. ) 
 CURVE ( )  GEOMETRIC_REPRESENTATION_ITEM ( )  RATIONAL_B_SPLINE_CURVE ( ( 1.000000000000000000, 0.9998288380325438540, 0.9998288380325438540, 1.000000000000000000 ) ) 
 REPRESENTATION_ITEM ( '' )  );
#2651 = CARTESIAN_POINT ( 'NONE',  ( 27.63948732994508006, 45.16218137147969003, 76.90433879953101837 ) ) ;
#2652 = LINE ( 'NONE', #9152, #12310 ) ;
#2653 = CARTESIAN_POINT ( 'NONE',  ( 2.436687528221640697, 49.84925249003585179, 77.23980501161587142 ) ) ;
#2654 = VECTOR ( 'NONE', #10381, 1000.000000000000000 ) ;
#2655 = CARTESIAN_POINT ( 'NONE',  ( 1.652727357819364418, 35.35299279957455099, 76.86610350541323555 ) ) ;
#2656 = CARTESIAN_POINT ( 'NONE',  ( -7.047195691697199393, 47.09221404848518944, 79.02985774836469091 ) ) ;
#2657 = LINE ( 'NONE', #12136, #9258 ) ;
#2658 = FACE_OUTER_BOUND ( 'NONE', #1926, .T. ) ;
#2659 = CARTESIAN_POINT ( 'NONE',  ( -3.533668833548938348, 36.21763952329489200, 78.50831005042292077 ) ) ;
#2660 = CARTESIAN_POINT ( 'NONE',  ( 23.03948732994508575, 45.16218137147969003, 78.60433879953099279 ) ) ;
#2661 = CARTESIAN_POINT ( 'NONE',  ( -2.013565751266337411, 38.84048690637051493, 95.03863327408461714 ) ) ;
#2662 = LINE ( 'NONE', #1382, #12497 ) ;
#2663 = LINE ( 'NONE', #20206, #14273 ) ;
#2664 = CARTESIAN_POINT ( 'NONE',  ( 35.92215374030650565, 40.96218137147972982, 93.55433879953098142 ) ) ;
#2665 = CIRCLE ( 'NONE', #14562, 0.9921021478795020165 ) ;
#2666 = CARTESIAN_POINT ( 'NONE',  ( 1.119863296874945791, 50.25084051303456789, 53.06567965797612629 ) ) ;
#2667 = ORIENTED_EDGE ( 'NONE', *, *, #3090, .F. ) ;
#2668 = CARTESIAN_POINT ( 'NONE',  ( 5.568489401881125289, 48.03437091500646261, 90.41433880123798872 ) ) ;
#2669 = CARTESIAN_POINT ( 'NONE',  ( 0.8336586891988152503, 52.35626390271237085, 78.71056005854129012 ) ) ;
#2670 = ORIENTED_EDGE ( 'NONE', *, *, #10386, .T. ) ;
#2671 = CARTESIAN_POINT ( 'NONE',  ( 0.7746764342352833177, 52.35878496689903017, 75.36252188568599308 ) ) ;
#2672 = VERTEX_POINT ( 'NONE', #8936 ) ;
#2673 = CARTESIAN_POINT ( 'NONE',  ( -4.437383981905837160, 50.68713408076344251, 78.75763390087725213 ) ) ;
#2674 = CARTESIAN_POINT ( 'NONE',  ( 5.544968037009670780, 45.50804040601273925, 93.69558880294498238 ) ) ;
#2675 = ORIENTED_EDGE ( 'NONE', *, *, #10607, .F. ) ;
#2676 = FACE_BOUND ( 'NONE', #2833, .T. ) ;
#2677 = AXIS2_PLACEMENT_3D ( 'NONE', #15887, #1308, #16095 ) ;
#2678 = CARTESIAN_POINT ( 'NONE',  ( -6.647464070959230753, 48.14170149837703860, 72.45433879953087342 ) ) ;
#2679 = CARTESIAN_POINT ( 'NONE',  ( -5.004817973257477348, 39.29348442311233214, 77.05433879953086773 ) ) ;
#2680 = PLANE ( 'NONE',  #8385 ) ;
#2681 =( LENGTH_UNIT ( ) NAMED_UNIT ( * ) SI_UNIT ( .MILLI., .METRE. ) );
#2682 = CARTESIAN_POINT ( 'NONE',  ( -4.811608766808351589, 37.16160227343304712, 79.54845644658969661 ) ) ;
#2683 = ORIENTED_EDGE ( 'NONE', *, *, #811, .F. ) ;
#2684 = LINE ( 'NONE', #20855, #13926 ) ;
#2685 = ORIENTED_EDGE ( 'NONE', *, *, #18602, .F. ) ;
#2686 = CARTESIAN_POINT ( 'NONE',  ( 23.63948732994508717, 36.35905713404684292, 74.70433879953098710 ) ) ;
#2687 = DIRECTION ( 'NONE',  ( 1.540237394707283727E-16, 1.793354297423763257E-16, -1.000000000000000000 ) ) ;
#2688 = CARTESIAN_POINT ( 'NONE',  ( 4.394343283833276992, 39.11584570990505938, 93.85183880123797451 ) ) ;
#2689 = EDGE_CURVE ( 'NONE', #4527, #20386, #7496, .T. ) ;
#2690 = DIRECTION ( 'NONE',  ( 1.000000000000000000, 1.402518428993831183E-16, -4.344610079045915326E-32 ) ) ;
#2691 = DIRECTION ( 'NONE',  ( 0.9485903129789527988, -0.3165065846431829311, 8.934458285744989980E-17 ) ) ;
#2692 = CARTESIAN_POINT ( 'NONE',  ( -4.396013154037729187, 37.60064804164377250, 77.91526691179548436 ) ) ;
#2693 = CARTESIAN_POINT ( 'NONE',  ( 5.601728273810613778, 37.72457639632248316, 78.37032190549847144 ) ) ;
#2694 = VECTOR ( 'NONE', #7470, 1000.000000000000000 ) ;
#2695 = ORIENTED_EDGE ( 'NONE', *, *, #4425, .F. ) ;
#2696 = CARTESIAN_POINT ( 'NONE',  ( 9.353599821682333726, 42.82705654907719151, 77.11956464767864361 ) ) ;
#2697 = ORIENTED_EDGE ( 'NONE', *, *, #10554, .T. ) ;
#2698 = VECTOR ( 'NONE', #3068, 1000.000000000000114 ) ;
#2699 = LINE ( 'NONE', #13666, #15975 ) ;
#2700 = ADVANCED_FACE ( 'NONE', ( #4130, #15530 ), #1168, .F. ) ;
#2701 = CARTESIAN_POINT ( 'NONE',  ( 6.198496396448986090, 45.68315280215533392, 92.99246380123798872 ) ) ;
#2702 = CARTESIAN_POINT ( 'NONE',  ( -7.840586881915256434, 41.40194303324297920, 78.11653805097020609 ) ) ;
#2703 = ORIENTED_EDGE ( 'NONE', *, *, #3654, .T. ) ;
#2704 = VECTOR ( 'NONE', #3356, 1000.000000000000000 ) ;
#2705 = CARTESIAN_POINT ( 'NONE',  ( -5.784195910403845176, 44.99242805365518194, 94.78933880123798872 ) ) ;
#2706 = CARTESIAN_POINT ( 'NONE',  ( -4.826313235042861471, 50.23618790873877060, 79.40394833312912226 ) ) ;
#2707 = DIRECTION ( 'NONE',  ( -1.540237394707284220E-16, -1.793354297423764243E-16, 1.000000000000000000 ) ) ;
#2708 = ORIENTED_EDGE ( 'NONE', *, *, #7274, .F. ) ;
#2709 = CARTESIAN_POINT ( 'NONE',  ( 6.882736312352589536, 37.89144858414100270, 77.26022115247205591 ) ) ;
#2710 = CARTESIAN_POINT ( 'NONE',  ( 5.561379608955574483, 51.38032281970146897, 76.39036821129558064 ) ) ;
#2711 = ADVANCED_FACE ( 'NONE', ( #9042 ), #5841, .T. ) ;
#2712 = ORIENTED_EDGE ( 'NONE', *, *, #17493, .F. ) ;
#2713 = CARTESIAN_POINT ( 'NONE',  ( 5.722153740306500147, 44.16218137147968292, 93.33161078214054385 ) ) ;
#2714 = CARTESIAN_POINT ( 'NONE',  ( -0.9988176903691428077, 49.83852402762217082, 90.80496380123797451 ) ) ;
#2715 = EDGE_LOOP ( 'NONE', ( #3482, #3305, #4945, #21020 ) ) ;
#2716 = CARTESIAN_POINT ( 'NONE',  ( 1.031158208426779410, 39.13855439321538654, 92.45433879953100131 ) ) ;
#2717 = CARTESIAN_POINT ( 'NONE',  ( -3.055882809522131094, 36.78399362325244937, 75.45433879953087342 ) ) ;
#2718 = CARTESIAN_POINT ( 'NONE',  ( 5.052198367669452850, 48.31320248322254685, 94.67308879782399345 ) ) ;
#2719 = VECTOR ( 'NONE', #15596, 1000.000000000000000 ) ;
#2720 = CARTESIAN_POINT ( 'NONE',  ( 5.316416202095706645, 37.50973464508803801, 75.36022115247205022 ) ) ;
#2721 = AXIS2_PLACEMENT_3D ( 'NONE', #16899, #2009, #19868 ) ;
#2722 = CARTESIAN_POINT ( 'NONE',  ( 8.787829143201870252, 41.13140593384865440, 76.40801527011910821 ) ) ;
#2723 = EDGE_CURVE ( 'NONE', #7833, #10210, #20614, .T. ) ;
#2724 = FACE_OUTER_BOUND ( 'NONE', #8996, .T. ) ;
#2725 = ORIENTED_EDGE ( 'NONE', *, *, #14942, .F. ) ;
#2726 = CARTESIAN_POINT ( 'NONE',  ( 2.058288634170412745, 52.20196483424038547, 76.07541412571639228 ) ) ;
#2727 = VECTOR ( 'NONE', #6762, 1000.000000000000000 ) ;
#2728 = AXIS2_PLACEMENT_3D ( 'NONE', #570, #14941, #10281 ) ;
#2729 = ORIENTED_EDGE ( 'NONE', *, *, #11455, .T. ) ;
#2730 = DIRECTION ( 'NONE',  ( 1.540237394707283727E-16, 1.793354297423763257E-16, -1.000000000000000000 ) ) ;
#2731 = CARTESIAN_POINT ( 'NONE',  ( 5.416600712022146880, 37.59071719501547193, 77.71701144737939160 ) ) ;
#2732 = CARTESIAN_POINT ( 'NONE',  ( 5.611423337425062385, 41.22389019960463230, 95.17996380123798872 ) ) ;
#2733 = B_SPLINE_SURFACE_WITH_KNOTS ( 'NONE', 3, 1, ( 
 ( #4722, #12730 ),
 ( #4836, #16237 ),
 ( #260, #13255 ),
 ( #1660, #6749 ),
 ( #10284, #8995 ),
 ( #3766, #15483 ),
 ( #15586, #10393 ),
 ( #894, #795 ),
 ( #11980, #7382 ),
 ( #10718, #2281 ),
 ( #13872, #16963 ),
 ( #8895, #12297 ),
 ( #17176, #1001 ),
 ( #15382, #20035 ),
 ( #16761, #7279 ),
 ( #19928, #15162 ),
 ( #573, #4695 ),
 ( #1320, #20867 ),
 ( #7804, #2702 ),
 ( #7704, #6297 ),
 ( #11017, #5902 ),
 ( #1528, #19089 ),
 ( #11117, #13985 ),
 ( #14290, #11221 ),
 ( #1215, #17385 ),
 ( #1115, #7908 ),
 ( #18878, #12798 ) ),
 .UNSPECIFIED., .F., .F., .F.,
 ( 4, 1, 1, 1, 1, 1, 1, 1, 1, 1, 1, 1, 1, 1, 1, 1, 1, 1, 1, 1, 1, 1, 1, 1, 4 ),
 ( 2, 2 ),
 ( 0.000000000000000000, 0.07935366776402412448, 0.1548335512306962258, 0.2264778788879675819, 0.2937702508597817563, 0.3573743676598307717, 0.4169588998156444348, 0.4725242949814433824, 0.5240711055231918047, 0.5716000239151953766, 0.6154428185654550187, 0.6549388753896664417, 0.6907509128113638042, 0.7224122923534581631, 0.7502020185738895730, 0.7741815239783794711, 0.7939676610466723794, 0.8283228184009381323, 0.8602605685341977448, 0.8894181639262210837, 0.9162808273808505932, 0.9404180486131810124, 0.9623203467589012128, 0.9822441917195737782, 0.9999999999999998890 ),
 ( 0.000000000000000000, 1.000000000000000000 ),
 .UNSPECIFIED. ) ;
#2734 = CARTESIAN_POINT ( 'NONE',  ( -3.715078426196892991, 51.18328438983323281, 75.42494517787103803 ) ) ;
#2735 = ORIENTED_EDGE ( 'NONE', *, *, #14052, .T. ) ;
#2736 = VECTOR ( 'NONE', #13308, 1000.000000000000000 ) ;
#2737 = CARTESIAN_POINT ( 'NONE',  ( -3.815104224344752382, 36.42552450956669219, 75.61442449207443417 ) ) ;
#2738 = CARTESIAN_POINT ( 'NONE',  ( -5.395897241545734246, 49.83815834233242015, 76.36688022495927441 ) ) ;
#2739 = VERTEX_POINT ( 'NONE', #6043 ) ;
#2740 = CARTESIAN_POINT ( 'NONE',  ( 4.611645699796032893, 52.08185300078213942, 78.81874598975664981 ) ) ;
#2741 = CARTESIAN_POINT ( 'NONE',  ( -0.4699484075729998822, 52.36218137147968577, 83.03825919817350609 ) ) ;
#2742 = CARTESIAN_POINT ( 'NONE',  ( 0.2860873169776717573, 38.75537135769874197, 91.15746379953097289 ) ) ;
#2743 = VERTEX_POINT ( 'NONE', #2651 ) ;
#2744 = CARTESIAN_POINT ( 'NONE',  ( 5.481509524342429884, 37.63185606553125240, 77.59973382626697003 ) ) ;
#2745 = CARTESIAN_POINT ( 'NONE',  ( -6.721170549555291807, 40.34851694082927764, 78.82487260570216847 ) ) ;
#2746 = CARTESIAN_POINT ( 'NONE',  ( -0.9376663952598962570, 52.84025806911358103, 76.73514787659645719 ) ) ;
#2747 = CARTESIAN_POINT ( 'NONE',  ( -0.9988176903691428077, 49.83852402762217082, 95.64871380123798872 ) ) ;
#2748 = VECTOR ( 'NONE', #2035, 1000.000000000000000 ) ;
#2749 = DIRECTION ( 'NONE',  ( -1.540237394707283727E-16, -1.793354297423763257E-16, 1.000000000000000000 ) ) ;
#2750 = EDGE_CURVE ( 'NONE', #5849, #14686, #9689, .T. ) ;
#2751 = LINE ( 'NONE', #12538, #345 ) ;
#2752 = ADVANCED_BREP_SHAPE_REPRESENTATION ( '', ( #4882, #18366 ), #20720 ) ;
#2753 = ADVANCED_FACE ( 'NONE', ( #14132 ), #10758, .T. ) ;
#2754 = CARTESIAN_POINT ( 'NONE',  ( -0.8237052942265477018, 49.18499566818285018, 92.75808880294498238 ) ) ;
#2755 = CARTESIAN_POINT ( 'NONE',  ( -4.964211958109541634, 43.56811128349716000, 78.65179900065426466 ) ) ;
#2756 = ADVANCED_FACE ( 'NONE', ( #7544 ), #17223, .T. ) ;
#2757 = CARTESIAN_POINT ( 'NONE',  ( 8.374483959044606962, 41.81265978262165817, 78.64183653779139149 ) ) ;
#2758 = EDGE_CURVE ( 'NONE', #20573, #16680, #14026, .T. ) ;
#2759 = CARTESIAN_POINT ( 'NONE',  ( -4.677846259693495767, 44.16218127507053737, 93.01911326394946400 ) ) ;
#2760 = B_SPLINE_CURVE_WITH_KNOTS ( 'NONE', 3,
 ( #14528, #3457, #13252, #19520, #10067, #14739 ),
 .UNSPECIFIED., .F., .F.,
 ( 4, 2, 4 ),
 ( 0.000000000000000000, 0.001346084890031584453, 0.002692169780063168906 ),
 .UNSPECIFIED. ) ;
#2761 = LINE ( 'NONE', #13817, #4382 ) ;
#2762 = CARTESIAN_POINT ( 'NONE',  ( 5.544968037009670780, 45.50804040601273925, 93.38308879953099506 ) ) ;
#2763 = CARTESIAN_POINT ( 'NONE',  ( 8.388854304654358884, 39.93565303222995055, 78.40165754912887053 ) ) ;
#2764 = CARTESIAN_POINT ( 'NONE',  ( 11.32022995165975843, 49.36218137147968577, 93.55433879953098142 ) ) ;
#2765 = EDGE_CURVE ( 'NONE', #8464, #2084, #14233, .T. ) ;
#2766 = CARTESIAN_POINT ( 'NONE',  ( -7.889836807277443853, 41.56303039276833289, 79.54845644658969661 ) ) ;
#2767 = DIRECTION ( 'NONE',  ( -1.571217453038212812E-16, -0.7071067811865500152, -0.7071067811865451302 ) ) ;
#2768 = VERTEX_POINT ( 'NONE', #7327 ) ;
#2769 = CARTESIAN_POINT ( 'NONE',  ( 8.632693788391325285, 43.03087348439100879, 78.75800315165874110 ) ) ;
#2770 = CARTESIAN_POINT ( 'NONE',  ( -4.032264951078912141, 50.98107207184723677, 76.47051527011910821 ) ) ;
#2771 = CARTESIAN_POINT ( 'NONE',  ( -5.004817973257478236, 39.29348442311233214, 78.53742703482498655 ) ) ;
#2772 = CARTESIAN_POINT ( 'NONE',  ( -1.477846259693489372, 49.76218137147969856, 53.55433879953100273 ) ) ;
#2773 = DIRECTION ( 'NONE',  ( 0.5813877811927011807, -0.8136266022444372803, -5.636455622144619183E-17 ) ) ;
#2774 = CIRCLE ( 'NONE', #17047, 4.200000000000003730 ) ;
#2775 = CYLINDRICAL_SURFACE ( 'NONE', #17003, 4.999999999999997335 ) ;
#2776 = DIRECTION ( 'NONE',  ( -0.5941461771851693774, -0.8043570849667760481, -2.357623395011396791E-16 ) ) ;
#2777 = CIRCLE ( 'NONE', #1402, 1.399999999999995026 ) ;
#2778 =( BOUNDED_CURVE ( )  B_SPLINE_CURVE ( 3, ( #19908, #5332, #15034, #13436 ),
 .UNSPECIFIED., .F., .F. ) 
 B_SPLINE_CURVE_WITH_KNOTS ( ( 4, 4 ),
 ( 5.988669822071448046, 6.577700792287722642 ),
 .UNSPECIFIED. ) 
 CURVE ( )  GEOMETRIC_REPRESENTATION_ITEM ( )  RATIONAL_B_SPLINE_CURVE ( ( 1.000000000000000000, 0.9712952651971044071, 0.9712952651971044071, 1.000000000000000000 ) ) 
 REPRESENTATION_ITEM ( '' )  );
#2779 = ORIENTED_EDGE ( 'NONE', *, *, #1332, .T. ) ;
#2780 = EDGE_CURVE ( 'NONE', #13982, #19239, #2761, .T. ) ;
#2781 = CARTESIAN_POINT ( 'NONE',  ( 3.460444912181559474, 49.25145096859824889, 91.74246380123798872 ) ) ;
#2782 = DIRECTION ( 'NONE',  ( 1.016439536705157818E-16, 1.000000000000000000, 0.000000000000000000 ) ) ;
#2783 = CARTESIAN_POINT ( 'NONE',  ( 5.766510840975054286, 51.22880064179873472, 78.93606911575150775 ) ) ;
#2784 = CARTESIAN_POINT ( 'NONE',  ( 5.579255781724441476, 50.61248246897039138, 76.90580938776616904 ) ) ;
#2785 = ORIENTED_EDGE ( 'NONE', *, *, #10699, .F. ) ;
#2786 = CIRCLE ( 'NONE', #6173, 0.5999999999999928724 ) ;
#2787 = CARTESIAN_POINT ( 'NONE',  ( 5.748274343403736886, 51.24227120794373747, 77.94845644658968808 ) ) ;
#2788 = AXIS2_PLACEMENT_3D ( 'NONE', #1345, #19415, #8041 ) ;
#2789 = CARTESIAN_POINT ( 'NONE',  ( -0.8237052942265477018, 49.18499566818285018, 92.75808880294498238 ) ) ;
#2790 = ORIENTED_EDGE ( 'NONE', *, *, #12998, .F. ) ;
#2791 = DIRECTION ( 'NONE',  ( 1.000000000000000000, 1.402518428993831676E-16, 0.000000000000000000 ) ) ;
#2792 = CARTESIAN_POINT ( 'NONE',  ( -0.9367543186758918727, 52.97864466936303529, 76.89011419028814487 ) ) ;
#2793 = CARTESIAN_POINT ( 'NONE',  ( 0.5221537403065010796, 44.16218137147969003, 77.84651775085080772 ) ) ;
#2794 = CARTESIAN_POINT ( 'NONE',  ( 28.43948732994508788, 36.35905713404685002, 74.70433879953100131 ) ) ;
#2795 = FACE_OUTER_BOUND ( 'NONE', #6961, .T. ) ;
#2796 = CARTESIAN_POINT ( 'NONE',  ( -3.597291554029906191, 36.26463506403467107, 78.92082147625116306 ) ) ;
#2797 = ORIENTED_EDGE ( 'NONE', *, *, #17800, .T. ) ;
#2798 = DIRECTION ( 'NONE',  ( 0.2741027427660463478, 0.8215033088236062264, -0.4999999999999973910 ) ) ;
#2799 = ORIENTED_EDGE ( 'NONE', *, *, #1657, .F. ) ;
#2800 = CARTESIAN_POINT ( 'NONE',  ( -7.244367111870785081, 46.79357224500207479, 79.23461367391459476 ) ) ;
#2801 = DIRECTION ( 'NONE',  ( 3.893792155548169402E-16, 7.183611964723547524E-17, -1.000000000000000000 ) ) ;
#2802 = CIRCLE ( 'NONE', #8578, 3.999999999999996447 ) ;
#2803 = DIRECTION ( 'NONE',  ( -0.8136266022444372803, -0.5813877811927012917, -2.295812393977109100E-16 ) ) ;
#2804 = LINE ( 'NONE', #1623, #7883 ) ;
#2805 = AXIS2_PLACEMENT_3D ( 'NONE', #14505, #6619, #20973 ) ;
#2806 = VERTEX_POINT ( 'NONE', #19034 ) ;
#2807 = CARTESIAN_POINT ( 'NONE',  ( 9.348820989215322896, 42.81273408501008504, 77.37738884012668450 ) ) ;
#2808 = ORIENTED_EDGE ( 'NONE', *, *, #3654, .F. ) ;
#2809 = CARTESIAN_POINT ( 'NONE',  ( -2.918372561058340864, 51.59970387748519727, 76.50206692849373269 ) ) ;
#2810 = CARTESIAN_POINT ( 'NONE',  ( -4.524181921268124462, 40.28999182795290324, 93.69558880123800293 ) ) ;
#2811 = CARTESIAN_POINT ( 'NONE',  ( 2.916646314871006229, 38.79555996194933698, 95.05433879953095300 ) ) ;
#2812 = ORIENTED_EDGE ( 'NONE', *, *, #3395, .T. ) ;
#2813 = EDGE_CURVE ( 'NONE', #4756, #6140, #6430, .T. ) ;
#2814 = CARTESIAN_POINT ( 'NONE',  ( -5.435385416347992660, 50.72091422709593189, 79.30596685730465367 ) ) ;
#2815 = CARTESIAN_POINT ( 'NONE',  ( 2.522153740306506631, 47.62628298661744708, 74.55433879953100984 ) ) ;
#2816 = CARTESIAN_POINT ( 'NONE',  ( -4.517608495229000098, 36.94443611587072240, 78.61392107264721574 ) ) ;
#2817 = CARTESIAN_POINT ( 'NONE',  ( 5.581171587375775900, 51.36570328251199413, 76.09992453055346573 ) ) ;
#2818 = AXIS2_PLACEMENT_3D ( 'NONE', #13477, #19854, #6773 ) ;
#2819 = ORIENTED_EDGE ( 'NONE', *, *, #2214, .T. ) ;
#2820 = CARTESIAN_POINT ( 'NONE',  ( -4.677846259693498432, 44.16218137147969003, 92.70661078214052964 ) ) ;
#2821 = CARTESIAN_POINT ( 'NONE',  ( 5.568489401881125289, 48.03437091500646261, 91.82058880123797451 ) ) ;
#2822 = VERTEX_POINT ( 'NONE', #10966 ) ;
#2823 = CARTESIAN_POINT ( 'NONE',  ( -4.862798738283528266, 42.89955397074594146, 92.45433879953101552 ) ) ;
#2824 = CARTESIAN_POINT ( 'NONE',  ( 6.004165720785556104, 44.16394627378592475, 95.05433879953098142 ) ) ;
#2825 = CARTESIAN_POINT ( 'NONE',  ( -4.812088799398938299, 42.22067586467031930, 91.46996379782397923 ) ) ;
#2826 = EDGE_CURVE ( 'NONE', #3959, #17717, #5726, .T. ) ;
#2827 = CARTESIAN_POINT ( 'NONE',  ( 5.085584811987322595, 37.35418535211618263, 76.29939265556315320 ) ) ;
#2828 = CARTESIAN_POINT ( 'NONE',  ( 30.43948732994509143, 36.35905713404685002, 76.90433879953101837 ) ) ;
#2829 = VECTOR ( 'NONE', #14914, 1000.000000000000000 ) ;
#2830 = CARTESIAN_POINT ( 'NONE',  ( -3.847049756032941303, 36.44912138698024506, 77.64672866243046201 ) ) ;
#2831 = ORIENTED_EDGE ( 'NONE', *, *, #1275, .T. ) ;
#2832 = FACE_OUTER_BOUND ( 'NONE', #20366, .T. ) ;
#2833 = EDGE_LOOP ( 'NONE', ( #14116, #261, #8428, #8236, #19876, #764 ) ) ;
#2834 = CARTESIAN_POINT ( 'NONE',  ( 4.512269934384613990, 47.81844922806527620, 92.87621379953098710 ) ) ;
#2835 = CARTESIAN_POINT ( 'NONE',  ( -0.7999275206693371443, 52.25527902654923906, 75.91237294090058185 ) ) ;
#2836 = CARTESIAN_POINT ( 'NONE',  ( -0.3080929418689875576, 37.85583172076933778, 94.94558880123797451 ) ) ;
#2837 = B_SPLINE_CURVE_WITH_KNOTS ( 'NONE', 3,
 ( #6820, #13326, #19798, #3315, #15025, #3422, #442, #6924, #11634, #9821, #18110, #16308, #8217, #127, #13112, #3530 ),
 .UNSPECIFIED., .F., .F.,
 ( 4, 2, 2, 2, 2, 2, 2, 4 ),
 ( 0.000000000000000000, 0.0002686153547044001721, 0.0005372307094088003441, 0.001074461418817601989, 0.001343076773521993976, 0.001611692128226385962, 0.001880307482930778165, 0.002148922837635170151 ),
 .UNSPECIFIED. ) ;
#2838 = CARTESIAN_POINT ( 'NONE',  ( -3.970323366337335180, 51.02496109656326695, 75.37033317797633458 ) ) ;
#2839 = ORIENTED_EDGE ( 'NONE', *, *, #6356, .T. ) ;
#2840 = EDGE_LOOP ( 'NONE', ( #15503, #3531, #2152, #19912 ) ) ;
#2841 = EDGE_CURVE ( 'NONE', #279, #17248, #12232, .T. ) ;
#2842 = CARTESIAN_POINT ( 'NONE',  ( -4.320790804570143528, 36.79905481608120965, 75.39293290059653430 ) ) ;
#2843 = CARTESIAN_POINT ( 'NONE',  ( -6.828828674771580509, 40.52810780656849943, 77.72183404180550781 ) ) ;
#2844 = ORIENTED_EDGE ( 'NONE', *, *, #4355, .T. ) ;
#2845 = CARTESIAN_POINT ( 'NONE',  ( 4.833451453752482863, 51.91801402521529241, 79.26957207196610966 ) ) ;
#2846 = CARTESIAN_POINT ( 'NONE',  ( -1.077846259693492126, 50.16218137147969713, 53.55433879953100273 ) ) ;
#2847 = CARTESIAN_POINT ( 'NONE',  ( 7.741105926769938250, 40.37549481084163716, 75.80967849220077426 ) ) ;
#2848 = CIRCLE ( 'NONE', #8629, 3.999999999999996447 ) ;
#2849 = ORIENTED_EDGE ( 'NONE', *, *, #12126, .F. ) ;
#2850 = CARTESIAN_POINT ( 'NONE',  ( -4.537329489133271387, 36.95900321965770985, 78.11020518223413944 ) ) ;
#2851 = CARTESIAN_POINT ( 'NONE',  ( 5.847431522242757751, 51.16902779423016767, 77.98758453411963387 ) ) ;
#2852 = PLANE ( 'NONE',  #12243 ) ;
#2853 = CARTESIAN_POINT ( 'NONE',  ( 6.828503391016846891, 43.33193468930419101, 95.25808880123800293 ) ) ;
#2854 = EDGE_CURVE ( 'NONE', #10889, #15617, #12898, .T. ) ;
#2855 = CARTESIAN_POINT ( 'NONE',  ( 6.198133899858643936, 38.24375437806406808, 78.20706894449375568 ) ) ;
#2856 = ADVANCED_FACE ( 'NONE', ( #4750 ), #1799, .F. ) ;
#2857 = DIRECTION ( 'NONE',  ( -4.731737692062910312E-17, 0.7071067811865460184, 0.7071067811865490160 ) ) ;
#2858 = CARTESIAN_POINT ( 'NONE',  ( 0.5221537403065015237, 44.16218137147968292, 75.45433879953088763 ) ) ;
#2859 = CARTESIAN_POINT ( 'NONE',  ( -0.9273978588864755235, 52.97979615060394565, 78.43306491891449639 ) ) ;
#2860 = ORIENTED_EDGE ( 'NONE', *, *, #17431, .F. ) ;
#2861 = DIRECTION ( 'NONE',  ( -3.893792155548169402E-16, -7.183611964723547524E-17, 1.000000000000000000 ) ) ;
#2862 = CARTESIAN_POINT ( 'NONE',  ( 0.5868117437017631444, 52.36192644938283536, 77.38375056423674891 ) ) ;
#2863 = CARTESIAN_POINT ( 'NONE',  ( 8.807144941123576487, 41.18929660559136607, 79.54516904849367620 ) ) ;
#2864 = CARTESIAN_POINT ( 'NONE',  ( -3.350035803220276609, 49.20851703305431357, 90.88308880123797451 ) ) ;
#2865 = EDGE_CURVE ( 'NONE', #13992, #10817, #3072, .T. ) ;
#2866 = ADVANCED_FACE ( 'NONE', ( #1480 ), #16260, .F. ) ;
#2867 = ORIENTED_EDGE ( 'NONE', *, *, #17069, .F. ) ;
#2868 = CARTESIAN_POINT ( 'NONE',  ( -8.299466572873484438, 42.85840835471202581, 78.79856413697085316 ) ) ;
#2869 = DIRECTION ( 'NONE',  ( 1.000000000000000000, 0.000000000000000000, 0.000000000000000000 ) ) ;
#2870 = EDGE_CURVE ( 'NONE', #5518, #20498, #19545, .T. ) ;
#2871 = VERTEX_POINT ( 'NONE', #4550 ) ;
#2872 = CARTESIAN_POINT ( 'NONE',  ( 8.643936145691096584, 43.06456754242027074, 78.41904468188381827 ) ) ;
#2873 = CARTESIAN_POINT ( 'NONE',  ( -3.736319852780221495, 36.36732966792005328, 79.18890841331918296 ) ) ;
#2874 = EDGE_CURVE ( 'NONE', #20695, #6977, #11889, .T. ) ;
#2875 = LINE ( 'NONE', #6160, #9956 ) ;
#2877 = EDGE_CURVE ( 'NONE', #5038, #9071, #4859, .T. ) ;
#2876 = CARTESIAN_POINT ( 'NONE',  ( -3.539401246598059991, 43.09270903039240608, 82.45433879953087342 ) ) ;
#2878 = LINE ( 'NONE', #20625, #15552 ) ;
#2879 = CARTESIAN_POINT ( 'NONE',  ( 9.054037327392332912, 41.92924874979977545, 78.13567616980381558 ) ) ;
#2880 = CARTESIAN_POINT ( 'NONE',  ( 2.538045550429134600, 49.87014351810298507, 72.45432679953087529 ) ) ;
#2881 = CARTESIAN_POINT ( 'NONE',  ( 6.961907239250668233, 50.34580947589670075, 76.63889762306028786 ) ) ;
#2882 = EDGE_CURVE ( 'NONE', #11984, #3927, #7966, .T. ) ;
#2883 = CARTESIAN_POINT ( 'NONE',  ( -0.3080929418689875576, 37.85583172076933778, 92.44558880123798872 ) ) ;
#2884 = CARTESIAN_POINT ( 'NONE',  ( -5.171864905379679023, 50.90921633613218944, 79.44348587025405095 ) ) ;
#2885 = CARTESIAN_POINT ( 'NONE',  ( 5.666494898543479763, 37.02236699927324537, 78.30432351818811298 ) ) ;
#2886 = VERTEX_POINT ( 'NONE', #19442 ) ;
#2887 = DIRECTION ( 'NONE',  ( 1.000000000000000000, 0.000000000000000000, 0.000000000000000000 ) ) ;
#2888 = ADVANCED_FACE ( 'NONE', ( #17750 ), #19331, .F. ) ;
#2889 = CARTESIAN_POINT ( 'NONE',  ( -5.058133621542618030, 44.89684013992257405, 94.24246380294498238 ) ) ;
#2890 = ORIENTED_EDGE ( 'NONE', *, *, #7439, .T. ) ;
#2891 = CARTESIAN_POINT ( 'NONE',  ( 5.895605937740185709, 51.13344329408603528, 78.75475733230618403 ) ) ;
#2892 = CARTESIAN_POINT ( 'NONE',  ( -0.9434902559443921755, 52.21950436431747278, 77.15777051809955367 ) ) ;
#2893 = CARTESIAN_POINT ( 'NONE',  ( 5.196643236000038080, 51.64973888592641771, 79.48101422306089603 ) ) ;
#2894 = LINE ( 'NONE', #15879, #18233 ) ;
#2895 = CARTESIAN_POINT ( 'NONE',  ( 0.5892521710836133852, 52.35418392935860510, 75.97241503363285631 ) ) ;
#2896 = EDGE_CURVE ( 'NONE', #15717, #3265, #3180, .T. ) ;
#2897 = CARTESIAN_POINT ( 'NONE',  ( -4.069601230858995500, 36.61351119651401120, 79.44037905412795908 ) ) ;
#2898 = VERTEX_POINT ( 'NONE', #6151 ) ;
#2899 =( BOUNDED_CURVE ( )  B_SPLINE_CURVE ( 3, ( #4220, #7529, #8811, #13703 ),
 .UNSPECIFIED., .F., .F. ) 
 B_SPLINE_CURVE_WITH_KNOTS ( ( 4, 4 ),
 ( 2.801755744135676629, 3.481429563043917152 ),
 .UNSPECIFIED. ) 
 CURVE ( )  GEOMETRIC_REPRESENTATION_ITEM ( )  RATIONAL_B_SPLINE_CURVE ( ( 1.000000000000000000, 0.9618726943880426816, 0.9618726943880426816, 1.000000000000000000 ) ) 
 REPRESENTATION_ITEM ( '' )  );
#2900 = LINE ( 'NONE', #11200, #8496 ) ;
#2901 = B_SPLINE_CURVE_WITH_KNOTS ( 'NONE', 3,
 ( #19037, #14134, #12754, #16060, #20616, #7756, #6045, #19233, #9365, #6153, #1586, #12658, #14235, #4752, #19141 ),
 .UNSPECIFIED., .F., .F.,
 ( 4, 1, 1, 1, 1, 1, 1, 1, 1, 1, 1, 1, 4 ),
 ( 0.000000000000000000, 0.1100843045400305420, 0.2037028897711227471, 0.2865965782701816456, 0.3664837514983516065, 0.4113922274074651164, 0.4651658430714658010, 0.5281943374952151604, 0.6014928947756199573, 0.6850328536222562992, 0.7789954854465236389, 0.8848457782734755472, 1.000000000000000000 ),
 .UNSPECIFIED. ) ;
#2902 = VERTEX_POINT ( 'NONE', #9572 ) ;
#2903 = CARTESIAN_POINT ( 'NONE',  ( -3.350035803220276609, 49.20851703305431357, 93.22683880123798872 ) ) ;
#2904 = CARTESIAN_POINT ( 'NONE',  ( 23.03948732994508930, 27.61837231449496599, 76.90433879953101837 ) ) ;
#2905 = CARTESIAN_POINT ( 'NONE',  ( -1.077846259693497677, 50.16218137147969713, 85.55433879953100984 ) ) ;
#2906 = DIRECTION ( 'NONE',  ( -1.000000000000000000, -6.608470384673549446E-15, 0.000000000000000000 ) ) ;
#2907 = CARTESIAN_POINT ( 'NONE',  ( -7.361413977510151696, 41.92405526712225594, 78.79490040793942285 ) ) ;
#2908 = B_SPLINE_SURFACE_WITH_KNOTS ( 'NONE', 3, 1, ( 
 ( #1953, #4919 ),
 ( #1858, #146 ),
 ( #19816, #6625 ),
 ( #6731, #19604 ),
 ( #10054, #13235 ),
 ( #10159, #8445 ),
 ( #5238, #13129 ),
 ( #3549, #14925 ),
 ( #11854, #8343 ),
 ( #14825, #3648 ),
 ( #19714, #16641 ),
 ( #16329, #5132 ),
 ( #8238, #2060 ),
 ( #8555, #15043 ),
 ( #11652, #11440 ),
 ( #6939, #458 ),
 ( #13444, #6524 ),
 ( #17912, #3335 ),
 ( #2169, #3748 ),
 ( #19916, #9840 ),
 ( #5340, #18130 ),
 ( #18330, #10270 ),
 ( #16746, #46 ),
 ( #13031, #19505 ),
 ( #13655, #16951 ),
 ( #7264, #7044 ),
 ( #4068, #8668 ) ),
 .UNSPECIFIED., .F., .F., .F.,
 ( 4, 1, 1, 1, 1, 1, 1, 1, 1, 1, 1, 1, 1, 1, 1, 1, 1, 1, 1, 1, 1, 1, 1, 1, 4 ),
 ( 2, 2 ),
 ( 0.000000000000000000, 0.03008419796516914949, 0.06086558711599211746, 0.09255548834448126816, 0.1250230453031442313, 0.1589818606095132758, 0.1938610318241761332, 0.2303980278329116893, 0.2682253880681681468, 0.2893299372400329750, 0.3134124272828068825, 0.3409194378824745297, 0.3718003620435414991, 0.4059162288623138770, 0.4432730987006598955, 0.4838755806815719374, 0.5280884695239720372, 0.5753551328988536495, 0.6260749037380917148, 0.6800510712237001210, 0.7372563232514290910, 0.7979168342633055078, 0.8620069649650062837, 0.9293841258006002581, 1.000000000000000000 ),
 ( 0.000000000000000000, 1.000000000000000000 ),
 .UNSPECIFIED. ) ;
#2909 = ORIENTED_EDGE ( 'NONE', *, *, #16136, .F. ) ;
#2910 = CARTESIAN_POINT ( 'NONE',  ( 9.353817388681445522, 42.82770861117572281, 77.06316232894263862 ) ) ;
#2911 = ORIENTED_EDGE ( 'NONE', *, *, #12657, .T. ) ;
#2912 = CARTESIAN_POINT ( 'NONE',  ( -2.923053016356064404, 51.59635939549185935, 76.41354228756682687 ) ) ;
#2913 = CARTESIAN_POINT ( 'NONE',  ( 2.043125170982144745, 38.48583871533720213, 95.17996380123798872 ) ) ;
#2914 = CARTESIAN_POINT ( 'NONE',  ( 5.080928206799192992, 51.73521291671138300, 75.47011219584838670 ) ) ;
#2915 = ORIENTED_EDGE ( 'NONE', *, *, #12953, .T. ) ;
#2916 = CARTESIAN_POINT ( 'NONE',  ( 2.463659247115865814, 38.82793883177424732, 95.37621379782397923 ) ) ;
#2917 = ORIENTED_EDGE ( 'NONE', *, *, #12729, .T. ) ;
#2918 = CARTESIAN_POINT ( 'NONE',  ( -4.427139072037590495, 51.44137015048543304, 78.85744209785094938 ) ) ;
#2919 = ORIENTED_EDGE ( 'NONE', *, *, #8591, .F. ) ;
#2920 = CARTESIAN_POINT ( 'NONE',  ( -4.677846259693817288, 43.47758838402644699, 92.73325776475002158 ) ) ;
#2921 = CARTESIAN_POINT ( 'NONE',  ( 0.5978773219678675810, 52.35412866480164951, 78.93607282253582014 ) ) ;
#2922 = ORIENTED_EDGE ( 'NONE', *, *, #4025, .F. ) ;
#2923 = CARTESIAN_POINT ( 'NONE',  ( -1.960491745668696106, 39.53320219679883962, 92.45433879953097289 ) ) ;
#2924 = CARTESIAN_POINT ( 'NONE',  ( 2.916646314871006229, 38.79555996194933698, 95.05433879953095300 ) ) ;
#2925 = CARTESIAN_POINT ( 'NONE',  ( 5.052198367669454626, 48.31320248322254685, 92.17308879782397923 ) ) ;
#2926 = CARTESIAN_POINT ( 'NONE',  ( 5.304793302263878907, 37.51082371353273714, 75.97198585835440099 ) ) ;
#2927 = CARTESIAN_POINT ( 'NONE',  ( 8.831661421392389855, 41.26277405225351202, 75.98994273744924044 ) ) ;
#2928 = CARTESIAN_POINT ( 'NONE',  ( -3.356204558708832053, 37.01138675915414922, 77.61986069475027250 ) ) ;
#2929 = ORIENTED_EDGE ( 'NONE', *, *, #17038, .F. ) ;
#2930 = CARTESIAN_POINT ( 'NONE',  ( -7.079104428204942678, 47.23853788948614607, 78.28573025590448253 ) ) ;
#2931 = LINE ( 'NONE', #8538, #3105 ) ;
#2932 = ORIENTED_EDGE ( 'NONE', *, *, #12363, .T. ) ;
#2933 = CARTESIAN_POINT ( 'NONE',  ( 5.053692675489762642, 42.04909006277621586, 92.64183879953097289 ) ) ;
#2934 = CARTESIAN_POINT ( 'NONE',  ( 5.848554534127551108, 37.15246014923294382, 77.40928489470421425 ) ) ;
#2935 = CARTESIAN_POINT ( 'NONE',  ( 5.611423337425062385, 41.22389019960463230, 91.58621380123798872 ) ) ;
#2936 = CARTESIAN_POINT ( 'NONE',  ( -3.628814973742291894, 51.23455773969688920, 75.44858973835683003 ) ) ;
#2937 = EDGE_LOOP ( 'NONE', ( #7779, #13147, #20779, #15730, #1589 ) ) ;
#2938 = VERTEX_POINT ( 'NONE', #16058 ) ;
#2939 = CARTESIAN_POINT ( 'NONE',  ( -3.115596136743314482, 36.83365901014666122, 76.03954924220039402 ) ) ;
#2940 = CARTESIAN_POINT ( 'NONE',  ( -4.303842671124285424, 37.54117185462008877, 75.97486526700035370 ) ) ;
#2941 = CARTESIAN_POINT ( 'NONE',  ( -4.691270138005329216, 50.49220747607777326, 75.40225920472202858 ) ) ;
#2942 = EDGE_LOOP ( 'NONE', ( #13176, #3890, #11751, #3746, #429, #16731, #1444, #19901 ) ) ;
#2943 = CARTESIAN_POINT ( 'NONE',  ( -4.148395103613341739, 37.44647417508210197, 76.91875223014945107 ) ) ;
#2944 = CARTESIAN_POINT ( 'NONE',  ( 6.450247442662826458, 38.49669771550791353, 77.26022115247205591 ) ) ;
#2945 = CARTESIAN_POINT ( 'NONE',  ( 5.053692675489763531, 42.04909006277621586, 91.39183879953097289 ) ) ;
#2946 = AXIS2_PLACEMENT_3D ( 'NONE', #8906, #807, #7293 ) ;
#2947 = ORIENTED_EDGE ( 'NONE', *, *, #4287, .T. ) ;
#2948 = CARTESIAN_POINT ( 'NONE',  ( -4.717426356068883386, 37.09203352051872571, 77.92182307551118470 ) ) ;
#2949 = CARTESIAN_POINT ( 'NONE',  ( -7.466141682373640620, 40.21844209608204324, 79.01214282451080351 ) ) ;
#2950 = CARTESIAN_POINT ( 'NONE',  ( -5.094963349914481299, 38.18624571745164076, 79.46021242174440147 ) ) ;
#2951 = CARTESIAN_POINT ( 'NONE',  ( -4.567115856812060670, 47.10047254335474065, 93.46121380123797451 ) ) ;
#2952 = EDGE_CURVE ( 'NONE', #6298, #8901, #14451, .T. ) ;
#2953 = CARTESIAN_POINT ( 'NONE',  ( -5.569494948991628114, 50.62508446513216143, 75.69846806870741318 ) ) ;
#2954 = CARTESIAN_POINT ( 'NONE',  ( 0.5221537403064990812, 44.16218137147969003, 95.05433879953096721 ) ) ;
#2955 = PLANE ( 'NONE',  #14249 ) ;
#2956 = CARTESIAN_POINT ( 'NONE',  ( -0.9083001327017958815, 52.97964555801444675, 78.68934297065942474 ) ) ;
#2957 =( GEOMETRIC_REPRESENTATION_CONTEXT ( 3 ) GLOBAL_UNCERTAINTY_ASSIGNED_CONTEXT ( ( #2150 ) ) GLOBAL_UNIT_ASSIGNED_CONTEXT ( ( #2681, #6381, #20852 ) ) REPRESENTATION_CONTEXT ( 'NONE', 'WORKASPACE' ) );
#2958 = ORIENTED_EDGE ( 'NONE', *, *, #4670, .T. ) ;
#2959 = CARTESIAN_POINT ( 'NONE',  ( 0.5221537403065015237, 44.16218137147968292, 75.45433879953087342 ) ) ;
#2960 = CYLINDRICAL_SURFACE ( 'NONE', #17049, 0.5999999999999894307 ) ;
#2961 = CARTESIAN_POINT ( 'NONE',  ( 2.722153740306517911, 44.16218137147969003, 56.15433879953099705 ) ) ;
#2962 = CARTESIAN_POINT ( 'NONE',  ( 5.611423337425062385, 41.22389019960463230, 90.33621380123798872 ) ) ;
#2963 = EDGE_LOOP ( 'NONE', ( #9868, #6230, #2177, #20028 ) ) ;
#2964 = ADVANCED_FACE ( 'NONE', ( #3372, #16160 ), #8065, .F. ) ;
#2965 = ORIENTED_EDGE ( 'NONE', *, *, #18293, .F. ) ;
#2966 = CARTESIAN_POINT ( 'NONE',  ( 8.643644394765681582, 43.06369314638848778, 78.50890480505780999 ) ) ;
#2967 = LINE ( 'NONE', #11176, #8063 ) ;
#2968 = CARTESIAN_POINT ( 'NONE',  ( -4.705149740856862550, 37.08296527939383935, 78.93669174070734584 ) ) ;
#2970 = EDGE_CURVE ( 'NONE', #6925, #17824, #9853, .T. ) ;
#2969 = CARTESIAN_POINT ( 'NONE',  ( -1.077846259693496123, 49.76218137147969856, 77.55433879953099563 ) ) ;
#2971 = DIRECTION ( 'NONE',  ( -1.540237394707284220E-16, -1.793354297423764243E-16, 1.000000000000000000 ) ) ;
#2972 = VECTOR ( 'NONE', #4737, 1000.000000000000000 ) ;
#2973 = CARTESIAN_POINT ( 'NONE',  ( 6.420168591842209338, 49.82113704518689445, 77.39285358288198324 ) ) ;
#2974 = DIRECTION ( 'NONE',  ( 1.000000000000000000, -1.193617070626243484E-16, 0.000000000000000000 ) ) ;
#2975 = LINE ( 'NONE', #15967, #6569 ) ;
#2976 = EDGE_CURVE ( 'NONE', #13351, #16624, #19676, .T. ) ;
#2977 = EDGE_CURVE ( 'NONE', #2342, #19757, #6767, .T. ) ;
#2978 = CARTESIAN_POINT ( 'NONE',  ( 8.824963465026481657, 41.24269985211446254, 78.91056401563228917 ) ) ;
#2979 = VECTOR ( 'NONE', #11544, 1000.000000000000114 ) ;
#2980 = CARTESIAN_POINT ( 'NONE',  ( 0.8434211303427824324, 52.35588695112656410, 78.61836880615196321 ) ) ;
#2981 = EDGE_CURVE ( 'NONE', #6536, #16740, #13476, .T. ) ;
#2982 = CARTESIAN_POINT ( 'NONE',  ( 5.920503277122149299, 37.20387208676527280, 78.36928251986560667 ) ) ;
#2983 = VERTEX_POINT ( 'NONE', #18166 ) ;
#2984 = CARTESIAN_POINT ( 'NONE',  ( 3.099655065065782367, 37.00631057046153671, 72.45432679953087529 ) ) ;
#2985 = CARTESIAN_POINT ( 'NONE',  ( 3.948530577815480225, 39.69684013992245752, 92.21121380294495395 ) ) ;
#2986 = ORIENTED_EDGE ( 'NONE', *, *, #17560, .F. ) ;
#2987 = CARTESIAN_POINT ( 'NONE',  ( -2.825834663281995951, 48.16810349223128895, 95.03225227128623942 ) ) ;
#2988 = FACE_OUTER_BOUND ( 'NONE', #6607, .T. ) ;
#2989 = CARTESIAN_POINT ( 'NONE',  ( -4.423487203781090393, 50.70288581026932917, 76.07809204575713125 ) ) ;
#2990 = PLANE ( 'NONE',  #9061 ) ;
#2991 = CARTESIAN_POINT ( 'NONE',  ( 0.5221537403065015237, 44.16218137147968292, 75.45433879953088763 ) ) ;
#2992 = ORIENTED_EDGE ( 'NONE', *, *, #13629, .T. ) ;
#2993 = CARTESIAN_POINT ( 'NONE',  ( 2.484494565094238716, 50.04344131194920919, 78.25433879953088478 ) ) ;
#2994 = VECTOR ( 'NONE', #12633, 1000.000000000000000 ) ;
#2995 = ORIENTED_EDGE ( 'NONE', *, *, #178, .T. ) ;
#2996 = CARTESIAN_POINT ( 'NONE',  ( 3.460444912181559474, 49.25145096859824889, 95.49246380123798872 ) ) ;
#2997 = EDGE_CURVE ( 'NONE', #8207, #9962, #16785, .T. ) ;
#2998 = CARTESIAN_POINT ( 'NONE',  ( 8.648170029844120421, 43.06315486489794608, 72.45433879953087342 ) ) ;
#2999 = FACE_OUTER_BOUND ( 'NONE', #15063, .T. ) ;
#3000 = DIRECTION ( 'NONE',  ( 1.402518428993831183E-16, -1.000000000000000000, 3.469446951953617640E-16 ) ) ;
#3001 = EDGE_CURVE ( 'NONE', #2198, #20811, #19949, .T. ) ;
#3002 = CARTESIAN_POINT ( 'NONE',  ( -5.921523028668191913, 37.98145122859525458, 76.14635491738357587 ) ) ;
#3003 = EDGE_LOOP ( 'NONE', ( #11625, #3949, #9552, #17418 ) ) ;
#3004 = EDGE_CURVE ( 'NONE', #13604, #9419, #15083, .T. ) ;
#3005 = CARTESIAN_POINT ( 'NONE',  ( -5.486992102393413617, 39.49954625374182626, 75.45433879953087342 ) ) ;
#3006 = AXIS2_PLACEMENT_3D ( 'NONE', #4501, #7913, #17283 ) ;
#3007 = ADVANCED_FACE ( 'NONE', ( #11690, #2306 ), #5070, .T. ) ;
#3008 = EDGE_CURVE ( 'NONE', #14315, #14996, #6770, .T. ) ;
#3009 = EDGE_LOOP ( 'NONE', ( #14530, #10640, #12792 ) ) ;
#3010 = B_SPLINE_CURVE_WITH_KNOTS ( 'NONE', 3,
 ( #5732, #2553, #5847, #13824, #14137, #20303, #12447, #13934, #9048, #7550, #15536, #10553 ),
 .UNSPECIFIED., .F., .F.,
 ( 4, 2, 2, 2, 2, 4 ),
 ( 0.000000000000000000, 0.0004293312658746052364, 0.0008586625317492104729, 0.001073328164686520843, 0.001287993797623830997, 0.001717325063498451520 ),
 .UNSPECIFIED. ) ;
#3011 = CARTESIAN_POINT ( 'NONE',  ( -3.353456363966241138, 52.20858450364031000, 76.50206692849373269 ) ) ;
#3012 = CARTESIAN_POINT ( 'NONE',  ( 5.568489401881125289, 48.03437091500646261, 93.07058880123797451 ) ) ;
#3013 = CARTESIAN_POINT ( 'NONE',  ( 5.243485048422129147, 51.61513872599351771, 75.41617184184443090 ) ) ;
#3014 = ORIENTED_EDGE ( 'NONE', *, *, #11706, .T. ) ;
#3015 = CARTESIAN_POINT ( 'NONE',  ( -5.787187992231675793, 50.46952898668384790, 78.79017217825926878 ) ) ;
#3016 = CARTESIAN_POINT ( 'NONE',  ( -7.677846259693483333, 47.36218137147966445, 93.55433879953098142 ) ) ;
#3017 = CARTESIAN_POINT ( 'NONE',  ( -4.526015856129117942, 36.95064629469847972, 78.75608284215286403 ) ) ;
#3018 = CARTESIAN_POINT ( 'NONE',  ( 5.220526778983810345, 50.87746113280923765, 76.09992453055346573 ) ) ;
#3019 = LINE ( 'NONE', #3129, #1417 ) ;
#3020 = VERTEX_POINT ( 'NONE', #14762 ) ;
#3021 = CARTESIAN_POINT ( 'NONE',  ( -4.956284031279793112, 43.92723849310139883, 92.55433879953098142 ) ) ;
#3022 = CARTESIAN_POINT ( 'NONE',  ( 0.8455664302218980355, 52.35217554515582350, 78.52566232894263010 ) ) ;
#3023 = ORIENTED_EDGE ( 'NONE', *, *, #8303, .T. ) ;
#3024 = DIRECTION ( 'NONE',  ( -1.540237394707284220E-16, -1.793354297423764243E-16, 1.000000000000000000 ) ) ;
#3025 = CARTESIAN_POINT ( 'NONE',  ( 0.5221537403065006355, 48.36218137147969287, 96.05433879953096721 ) ) ;
#3026 = VECTOR ( 'NONE', #7581, 1000.000000000000227 ) ;
#3027 = CARTESIAN_POINT ( 'NONE',  ( 0.7608161506431847521, 52.95895884780778573, 78.87528306474457906 ) ) ;
#3028 = CARTESIAN_POINT ( 'NONE',  ( -5.616286711741430793, 44.43019146960381960, 95.14183879782397923 ) ) ;
#3029 = CONTEXT_DEPENDENT_SHAPE_REPRESENTATION ( #8865, #11420 ) ;
#3030 = CARTESIAN_POINT ( 'NONE',  ( 0.5221537403065104055, 40.36218137147969998, 46.15433879953098284 ) ) ;
#3031 = PLANE ( 'NONE',  #9852 ) ;
#3032 = CARTESIAN_POINT ( 'NONE',  ( 5.829595689320886009, 51.18220240553836931, 75.98827401121828018 ) ) ;
#3033 = ORIENTED_EDGE ( 'NONE', *, *, #14335, .F. ) ;
#3034 = EDGE_CURVE ( 'NONE', #9780, #14257, #9993, .T. ) ;
#3035 = CARTESIAN_POINT ( 'NONE',  ( 2.069300872037923789, 52.82512215700846525, 77.34613596266348168 ) ) ;
#3036 = DIRECTION ( 'NONE',  ( -0.5941461771851693774, -0.8043570849667760481, -2.357623395011396791E-16 ) ) ;
#3037 = VECTOR ( 'NONE', #248, 1000.000000000000000 ) ;
#3038 = ORIENTED_EDGE ( 'NONE', *, *, #10403, .F. ) ;
#3039 = CARTESIAN_POINT ( 'NONE',  ( -8.144617840030331735, 42.60233705719735298, 76.47068638765421156 ) ) ;
#3040 = CARTESIAN_POINT ( 'NONE',  ( -0.9190990356458662580, 52.23452979981542654, 76.25498568266576171 ) ) ;
#3041 = DIRECTION ( 'NONE',  ( 0.000000000000000000, 0.000000000000000000, -1.000000000000000000 ) ) ;
#3042 = CARTESIAN_POINT ( 'NONE',  ( 8.850491666625398324, 41.31920949178531544, 79.54734031390459847 ) ) ;
#3043 = ORIENTED_EDGE ( 'NONE', *, *, #106, .T. ) ;
#3044 = VECTOR ( 'NONE', #17333, 1000.000000000000000 ) ;
#3045 = CARTESIAN_POINT ( 'NONE',  ( -1.477846259693495146, 49.76218137147969856, 85.55433879953100984 ) ) ;
#3046 = ORIENTED_EDGE ( 'NONE', *, *, #2098, .T. ) ;
#3047 = CARTESIAN_POINT ( 'NONE',  ( -4.716387082485074878, 37.09126585098686490, 75.36022115247205022 ) ) ;
#3048 = FACE_OUTER_BOUND ( 'NONE', #16544, .T. ) ;
#3049 = CARTESIAN_POINT ( 'NONE',  ( -6.859512391284826371, 40.59060452047487644, 77.62511654548754336 ) ) ;
#3050 = ORIENTED_EDGE ( 'NONE', *, *, #6872, .F. ) ;
#3051 = CARTESIAN_POINT ( 'NONE',  ( -4.518657848439222136, 36.94521123081658232, 76.91875223014945107 ) ) ;
#3052 = CARTESIAN_POINT ( 'NONE',  ( -6.721036008677163665, 40.31817738747478330, 78.72633731078545338 ) ) ;
#3053 = CARTESIAN_POINT ( 'NONE',  ( -3.628867371436362621, 48.69222599884265179, 91.07933879782399345 ) ) ;
#3054 = CIRCLE ( 'NONE', #13243, 8.199999999999995737 ) ;
#3055 = AXIS2_PLACEMENT_3D ( 'NONE', #15100, #11707, #5513 ) ;
#3056 = ORIENTED_EDGE ( 'NONE', *, *, #7272, .F. ) ;
#3057 = CARTESIAN_POINT ( 'NONE',  ( -7.782451534811345439, 41.25123178438806093, 78.77893168383444333 ) ) ;
#3058 = SURFACE_STYLE_USAGE ( .BOTH. , #4637 ) ;
#3059 = DIRECTION ( 'NONE',  ( 0.000000000000000000, -1.000000000000000000, 3.469446951953617147E-16 ) ) ;
#3060 = CARTESIAN_POINT ( 'NONE',  ( 5.146043734657006041, 40.41782908280415398, 90.30634084312077903 ) ) ;
#3061 = DIRECTION ( 'NONE',  ( 1.000000000000000000, 0.000000000000000000, 0.000000000000000000 ) ) ;
#3062 = ADVANCED_FACE ( 'NONE', ( #13580 ), #5377, .T. ) ;
#3063 = CARTESIAN_POINT ( 'NONE',  ( 6.393340659266161019, 38.43765720549087206, 77.85582082558342165 ) ) ;
#3064 = VECTOR ( 'NONE', #13782, 1000.000000000000000 ) ;
#3065 = CARTESIAN_POINT ( 'NONE',  ( 9.271561067608034890, 45.68041113525027441, 79.47125056423675460 ) ) ;
#3066 = VECTOR ( 'NONE', #18774, 1000.000000000000000 ) ;
#3067 = CARTESIAN_POINT ( 'NONE',  ( 1.042984815895136252, 52.96245648330992140, 76.77289608131282250 ) ) ;
#3068 = DIRECTION ( 'NONE',  ( 0.003037711714694931939, -0.009606198427078794025, -0.9999492453416412019 ) ) ;
#3069 = CARTESIAN_POINT ( 'NONE',  ( -0.6082159309068581043, 52.21483855284596132, 79.21387586705148465 ) ) ;
#3070 = AXIS2_PLACEMENT_3D ( 'NONE', #13652, #20124, #12064 ) ;
#3071 = ORIENTED_EDGE ( 'NONE', *, *, #19129, .F. ) ;
#3072 = LINE ( 'NONE', #21021, #1705 ) ;
#3073 = CARTESIAN_POINT ( 'NONE',  ( -3.154801521863568325, 47.83913663364971569, 94.11286078555450274 ) ) ;
#3074 = CARTESIAN_POINT ( 'NONE',  ( 8.436128353966983795, 40.07733635702963682, 79.00897045670630803 ) ) ;
#3075 = DIRECTION ( 'NONE',  ( -1.110223024625156540E-16, -1.000000000000000000, -5.922860397471808077E-17 ) ) ;
#3076 = ORIENTED_EDGE ( 'NONE', *, *, #19255, .T. ) ;
#3077 = ORIENTED_EDGE ( 'NONE', *, *, #8887, .F. ) ;
#3078 = ADVANCED_FACE ( 'NONE', ( #16573 ), #8489, .F. ) ;
#3079 = CARTESIAN_POINT ( 'NONE',  ( -1.477846259693491593, 47.62628298661744708, 53.15433879953100416 ) ) ;
#3080 = CARTESIAN_POINT ( 'NONE',  ( 1.514255888186008425, 52.36218137147968577, 48.36106904222365444 ) ) ;
#3081 = CARTESIAN_POINT ( 'NONE',  ( -4.853223633226589229, 37.19234149890713326, 78.86751516113972116 ) ) ;
#3082 = CARTESIAN_POINT ( 'NONE',  ( 28.52215374030649997, 44.16218137147968292, 45.55433879953098852 ) ) ;
#3083 = LINE ( 'NONE', #14570, #18611 ) ;
#3084 = VECTOR ( 'NONE', #19462, 1000.000000000000000 ) ;
#3085 = CARTESIAN_POINT ( 'NONE',  ( -3.069519124378985886, 36.79039167325804272, 76.24341621876634179 ) ) ;
#3086 = CARTESIAN_POINT ( 'NONE',  ( 8.567695763276095278, 42.83607027972283987, 77.86785210695053649 ) ) ;
#3087 = CARTESIAN_POINT ( 'NONE',  ( 5.599231707071657738, 51.35236299959863970, 78.30875056423674607 ) ) ;
#3088 = CARTESIAN_POINT ( 'NONE',  ( 5.228220230638878974, 50.87731552598469875, 76.07147373344933783 ) ) ;
#3089 = ADVANCED_FACE ( 'NONE', ( #14975 ), #16471, .F. ) ;
#3090 = EDGE_CURVE ( 'NONE', #476, #889, #1965, .T. ) ;
#3091 = ORIENTED_EDGE ( 'NONE', *, *, #10308, .F. ) ;
#3092 = FACE_OUTER_BOUND ( 'NONE', #3618, .T. ) ;
#3093 = LINE ( 'NONE', #5963, #12965 ) ;
#3094 = CARTESIAN_POINT ( 'NONE',  ( 5.450944860649778789, 36.86834283398499679, 78.16244716952144245 ) ) ;
#3095 = ORIENTED_EDGE ( 'NONE', *, *, #6187, .T. ) ;
#3096 = LINE ( 'NONE', #14475, #11586 ) ;
#3097 = CARTESIAN_POINT ( 'NONE',  ( 8.389283321988518338, 39.93693882439677623, 76.47636794762235013 ) ) ;
#3098 = ORIENTED_EDGE ( 'NONE', *, *, #15241, .F. ) ;
#3099 = CARTESIAN_POINT ( 'NONE',  ( 5.556673069113441166, 37.86366792307473617, 75.38041148603002739 ) ) ;
#3100 = CARTESIAN_POINT ( 'NONE',  ( -4.429894154275758389, 50.69802490680864082, 76.10363940379099290 ) ) ;
#3101 = LINE ( 'NONE', #2794, #9744 ) ;
#3102 = CARTESIAN_POINT ( 'NONE',  ( 0.6249198533375087683, 52.35390267657594165, 75.97323462179006981 ) ) ;
#3103 = DIRECTION ( 'NONE',  ( 1.779391786395883536E-16, 5.922860397471806844E-17, -1.000000000000000000 ) ) ;
#3104 = ORIENTED_EDGE ( 'NONE', *, *, #9620, .F. ) ;
#3105 = VECTOR ( 'NONE', #8109, 1000.000000000000000 ) ;
#3106 = CARTESIAN_POINT ( 'NONE',  ( 5.848951923618479931, 37.15274410921379911, 77.37492703482499223 ) ) ;
#3107 = ORIENTED_EDGE ( 'NONE', *, *, #14826, .T. ) ;
#3108 = CARTESIAN_POINT ( 'NONE',  ( -5.784195910403845176, 44.99242805365518194, 95.88308880123798872 ) ) ;
#3109 = CARTESIAN_POINT ( 'NONE',  ( -2.416137431568557314, 39.07291177436112406, 93.61746380123797451 ) ) ;
#3110 = CARTESIAN_POINT ( 'NONE',  ( -0.1944850259765472933, 35.99355670886600933, 76.86610350541323555 ) ) ;
#3111 = CARTESIAN_POINT ( 'NONE',  ( 5.846647460608473956, 37.15109742431862827, 76.40678776405631822 ) ) ;
#3112 = EDGE_CURVE ( 'NONE', #531, #7336, #5924, .T. ) ;
#3113 = CARTESIAN_POINT ( 'NONE',  ( -7.908203753683241466, 41.62291835105061466, 78.91811502121268518 ) ) ;
#3114 = VECTOR ( 'NONE', #18035, 1000.000000000000000 ) ;
#3115 = VERTEX_POINT ( 'NONE', #15612 ) ;
#3116 = CARTESIAN_POINT ( 'NONE',  ( 4.588242150565980282, 52.09914025984591746, 78.23954818826248925 ) ) ;
#3117 = VECTOR ( 'NONE', #6905, 1000.000000000000227 ) ;
#3118 = ORIENTED_EDGE ( 'NONE', *, *, #418, .F. ) ;
#3119 = LINE ( 'NONE', #9622, #19045 ) ;
#3120 = CARTESIAN_POINT ( 'NONE',  ( -1.219503646467433589, 49.90383875825363447, 77.41268141275706682 ) ) ;
#3121 = CARTESIAN_POINT ( 'NONE',  ( 4.552447320970152589, 52.12558045856467004, 76.26690125110441443 ) ) ;
#3122 = ORIENTED_EDGE ( 'NONE', *, *, #17021, .T. ) ;
#3123 = ADVANCED_FACE ( 'NONE', ( #712 ), #7408, .F. ) ;
#3124 = CARTESIAN_POINT ( 'NONE',  ( -5.802311964739910621, 50.45872194965342317, 78.71528818263502103 ) ) ;
#3125 = DIRECTION ( 'NONE',  ( -1.000000000000000000, 0.000000000000000000, 0.000000000000000000 ) ) ;
#3126 = CARTESIAN_POINT ( 'NONE',  ( -4.260738562919781813, 37.50933258622881539, 78.92211507803222048 ) ) ;
#3127 = CARTESIAN_POINT ( 'NONE',  ( 5.561486116954087677, 51.38024414653337146, 76.36928804473561172 ) ) ;
#3128 = ADVANCED_FACE ( 'NONE', ( #10519 ), #5412, .T. ) ;
#3129 = CARTESIAN_POINT ( 'NONE',  ( -0.02883801100815608018, 35.36625256049322275, 79.45433879953087342 ) ) ;
#3130 = VERTEX_POINT ( 'NONE', #10937 ) ;
#3131 = CARTESIAN_POINT ( 'NONE',  ( -4.769179815246321397, 42.34626837109277631, 92.55433879953098142 ) ) ;
#3132 = PLANE ( 'NONE',  #1820 ) ;
#3133 = VECTOR ( 'NONE', #4125, 1000.000000000000000 ) ;
#3134 = ORIENTED_EDGE ( 'NONE', *, *, #17130, .F. ) ;
#3135 = CARTESIAN_POINT ( 'NONE',  ( 4.715683878568929011, 52.00500418903608590, 77.90619853385557292 ) ) ;
#3136 = CARTESIAN_POINT ( 'NONE',  ( 5.933406720878987350, 44.83544050270759840, 95.05433879953098142 ) ) ;
#3137 = DIRECTION ( 'NONE',  ( -0.7071067811865474617, 1.203855704449244074E-16, -0.7071067811865476838 ) ) ;
#3138 = EDGE_CURVE ( 'NONE', #6753, #4999, #13695, .T. ) ;
#3139 = VECTOR ( 'NONE', #7662, 1000.000000000000227 ) ;
#3140 = ADVANCED_FACE ( 'NONE', ( #919, #2418 ), #4312, .F. ) ;
#3141 = CARTESIAN_POINT ( 'NONE',  ( -6.210882734309923769, 46.73118581782181025, 77.58227997600145898 ) ) ;
#3142 = CARTESIAN_POINT ( 'NONE',  ( -3.628867371436363509, 48.69222599884265179, 92.48558879782397923 ) ) ;
#3143 = DIRECTION ( 'NONE',  ( 1.402518428993831676E-16, -1.000000000000000000, 0.000000000000000000 ) ) ;
#3144 = EDGE_CURVE ( 'NONE', #18072, #16704, #20225, .T. ) ;
#3145 = FACE_OUTER_BOUND ( 'NONE', #64, .T. ) ;
#3146 = CARTESIAN_POINT ( 'NONE',  ( 29.63948732994508006, 43.16218137147969003, 74.70433879953100131 ) ) ;
#3147 = ORIENTED_EDGE ( 'NONE', *, *, #19459, .F. ) ;
#3148 = CARTESIAN_POINT ( 'NONE',  ( 2.046000312423422507, 52.20206269949791533, 78.89969410769322167 ) ) ;
#3149 = VERTEX_POINT ( 'NONE', #2525 ) ;
#3150 = VECTOR ( 'NONE', #1218, 1000.000000000000000 ) ;
#3151 = LINE ( 'NONE', #9652, #7815 ) ;
#3152 = DIRECTION ( 'NONE',  ( 1.540237394707284220E-16, 1.793354297423764243E-16, -1.000000000000000000 ) ) ;
#3153 = CARTESIAN_POINT ( 'NONE',  ( 0.5221537403065118488, 48.16218137147969003, 45.55433879953100273 ) ) ;
#3154 = AXIS2_PLACEMENT_3D ( 'NONE', #8615, #294, #16380 ) ;
#3155 = LINE ( 'NONE', #17308, #11527 ) ;
#3156 = ORIENTED_EDGE ( 'NONE', *, *, #11419, .T. ) ;
#3157 = LINE ( 'NONE', #2655, #16332 ) ;
#3158 = VERTEX_POINT ( 'NONE', #9021 ) ;
#3159 = CARTESIAN_POINT ( 'NONE',  ( -7.866550369700228806, 41.50330127738815378, 78.93669174070734584 ) ) ;
#3160 = CARTESIAN_POINT ( 'NONE',  ( 8.378483041054197500, 41.81311971792333537, 78.53442867677860306 ) ) ;
#3161 = CARTESIAN_POINT ( 'NONE',  ( 1.868012774839550749, 39.13936707477651566, 93.07058879953099506 ) ) ;
#3162 = VERTEX_POINT ( 'NONE', #20381 ) ;
#3163 = CARTESIAN_POINT ( 'NONE',  ( 4.140412088821458170, 51.51591928153320765, 78.46169174070733732 ) ) ;
#3164 = CARTESIAN_POINT ( 'NONE',  ( 8.833159395675938441, 41.26726357621102181, 77.50846324053436831 ) ) ;
#3165 = CARTESIAN_POINT ( 'NONE',  ( 4.512269934384614878, 47.81844922806527620, 92.87621379953098710 ) ) ;
#3166 = AXIS2_PLACEMENT_3D ( 'NONE', #15274, #20361, #13675 ) ;
#3167 = ORIENTED_EDGE ( 'NONE', *, *, #6198, .F. ) ;
#3168 = FACE_OUTER_BOUND ( 'NONE', #1552, .T. ) ;
#3169 = CARTESIAN_POINT ( 'NONE',  ( -5.395909702104524364, 38.48590459560077903, 79.18739798713926348 ) ) ;
#3170 = EDGE_CURVE ( 'NONE', #10809, #122, #20796, .T. ) ;
#3171 = CARTESIAN_POINT ( 'NONE',  ( -4.524181921268124462, 40.28999182795290324, 92.44558880123798872 ) ) ;
#3172 = VECTOR ( 'NONE', #19858, 1000.000000000000000 ) ;
#3173 = CARTESIAN_POINT ( 'NONE',  ( 4.001626195812781006, 40.29782224849783745, 89.72723091094957226 ) ) ;
#3174 = CARTESIAN_POINT ( 'NONE',  ( -4.484214873741871443, 37.66782333187624943, 76.00985440664865678 ) ) ;
#3175 = CARTESIAN_POINT ( 'NONE',  ( 0.5234091789269255113, 52.34369878586026203, 76.89772265631788173 ) ) ;
#3176 = VERTEX_POINT ( 'NONE', #7727 ) ;
#3177 = LINE ( 'NONE', #11378, #12559 ) ;
#3178 = CARTESIAN_POINT ( 'NONE',  ( -0.4185253612809345936, 52.97578350394660163, 79.34012451928875009 ) ) ;
#3179 = ORIENTED_EDGE ( 'NONE', *, *, #9240, .F. ) ;
#3180 = LINE ( 'NONE', #20823, #13578 ) ;
#3181 = DIRECTION ( 'NONE',  ( -1.540237394707283727E-16, -1.793354297423763257E-16, 1.000000000000000000 ) ) ;
#3182 = CARTESIAN_POINT ( 'NONE',  ( 0.8448466153661705613, 52.35582950748954545, 76.37320713360470847 ) ) ;
#3183 = CARTESIAN_POINT ( 'NONE',  ( 2.026641451580078357, 52.83264100297040500, 78.95121740658819931 ) ) ;
#3184 = ORIENTED_EDGE ( 'NONE', *, *, #5323, .F. ) ;
#3185 = CARTESIAN_POINT ( 'NONE',  ( 7.688925413721245050, 40.17753638632645163, 76.35905954771017434 ) ) ;
#3186 = FILL_AREA_STYLE ('',( #1809 ) ) ;
#3187 = DIRECTION ( 'NONE',  ( 1.000000000000000000, -1.110223024625156417E-16, -1.111814006898795283E-16 ) ) ;
#3188 = CARTESIAN_POINT ( 'NONE',  ( 5.263499222790406051, 50.85473774294745652, 79.54645054556618788 ) ) ;
#3189 = PLANE ( 'NONE',  #4864 ) ;
#3190 = LINE ( 'NONE', #8294, #15904 ) ;
#3191 = CARTESIAN_POINT ( 'NONE',  ( -4.895593109503407092, 37.22363812428621088, 76.38448585835440952 ) ) ;
#3192 = CARTESIAN_POINT ( 'NONE',  ( 6.127581622321778276, 50.03725925344959080, 77.67636243622263237 ) ) ;
#3193 = DIRECTION ( 'NONE',  ( -0.5813877811927011807, 0.8136266022444372803, 5.636455622144619183E-17 ) ) ;
#3194 = VECTOR ( 'NONE', #4830, 1000.000000000000114 ) ;
#3195 = ORIENTED_EDGE ( 'NONE', *, *, #8884, .T. ) ;
#3196 = CARTESIAN_POINT ( 'NONE',  ( -4.364285939139664450, 37.76718941598996082, 79.54845644658969661 ) ) ;
#3197 = EDGE_CURVE ( 'NONE', #13434, #19503, #20992, .T. ) ;
#3198 = ORIENTED_EDGE ( 'NONE', *, *, #1718, .T. ) ;
#3199 = CARTESIAN_POINT ( 'NONE',  ( 8.951691408152598228, 41.62251153713423690, 78.44085888008430629 ) ) ;
#3200 = DIRECTION ( 'NONE',  ( -1.084202172485505420E-16, -1.000000000000000000, 0.000000000000000000 ) ) ;
#3201 = DIRECTION ( 'NONE',  ( 1.000000000000000000, 0.000000000000000000, 0.000000000000000000 ) ) ;
#3202 = CARTESIAN_POINT ( 'NONE',  ( 9.131267103411046193, 42.16071128789349132, 78.09998440036279987 ) ) ;
#3203 = ORIENTED_EDGE ( 'NONE', *, *, #1938, .F. ) ;
#3204 = CARTESIAN_POINT ( 'NONE',  ( 6.146933156575338231, 38.28544617077390200, 75.62429547252081363 ) ) ;
#3205 = CARTESIAN_POINT ( 'NONE',  ( 0.5221537403065117378, 47.36218137147970708, 45.55433879953100273 ) ) ;
#3206 = CARTESIAN_POINT ( 'NONE',  ( 6.032012598193956521, 38.20332814726474879, 78.28436300994860630 ) ) ;
#3207 = CARTESIAN_POINT ( 'NONE',  ( 9.539487329945091076, 44.16218137147970424, 95.45352954694192249 ) ) ;
#3208 = CARTESIAN_POINT ( 'NONE',  ( 0.7587367783518825792, 49.63488860465389507, 92.45433879953102974 ) ) ;
#3209 = ORIENTED_EDGE ( 'NONE', *, *, #14005, .F. ) ;
#3210 = CARTESIAN_POINT ( 'NONE',  ( 8.375199775097005528, 41.81478521990748476, 76.38301527011910252 ) ) ;
#3211 = VERTEX_POINT ( 'NONE', #7937 ) ;
#3212 = CARTESIAN_POINT ( 'NONE',  ( -0.9988176903691428077, 49.83852402762217082, 91.89871380123798872 ) ) ;
#3213 = CARTESIAN_POINT ( 'NONE',  ( -7.876156483970349953, 46.79098802322403117, 79.40730115154055113 ) ) ;
#3214 = DIRECTION ( 'NONE',  ( 0.007885122365275663500, 0.9999689119394085113, 1.805443505845543142E-16 ) ) ;
#3215 = CARTESIAN_POINT ( 'NONE',  ( 8.415751671997487193, 46.40539568610629573, 77.63812446857940586 ) ) ;
#3216 = EDGE_CURVE ( 'NONE', #13955, #17982, #6512, .T. ) ;
#3217 = EDGE_CURVE ( 'NONE', #5430, #9093, #1235, .T. ) ;
#3218 = VERTEX_POINT ( 'NONE', #1656 ) ;
#3219 = CARTESIAN_POINT ( 'NONE',  ( -4.525716193177017566, 36.95042494574692427, 76.22840587216694530 ) ) ;
#3220 = ORIENTED_EDGE ( 'NONE', *, *, #17025, .F. ) ;
#3221 = CARTESIAN_POINT ( 'NONE',  ( -3.350440871817599753, 52.21073926392551812, 76.59793576264409865 ) ) ;
#3222 = CARTESIAN_POINT ( 'NONE',  ( -5.784195910403845176, 44.99242805365518194, 91.03933880123798872 ) ) ;
#3223 = CARTESIAN_POINT ( 'NONE',  ( 0.5221537403065010796, 44.16218137147968292, 78.25433879953088478 ) ) ;
#3224 = ORIENTED_EDGE ( 'NONE', *, *, #3889, .F. ) ;
#3225 = CARTESIAN_POINT ( 'NONE',  ( 9.273778039597953438, 45.67340037358405169, 78.74919174070734584 ) ) ;
#3226 = CARTESIAN_POINT ( 'NONE',  ( -5.210464978622034060, 37.45622129019157853, 79.52089765539699329 ) ) ;
#3227 = CARTESIAN_POINT ( 'NONE',  ( 5.880020243381231637, 42.59485829234928644, 92.55433879953100984 ) ) ;
#3228 = EDGE_CURVE ( 'NONE', #3149, #11295, #6225, .T. ) ;
#3229 = LINE ( 'NONE', #16212, #19998 ) ;
#3230 = DIRECTION ( 'NONE',  ( 0.000000000000000000, 0.000000000000000000, 1.000000000000000000 ) ) ;
#3231 = ORIENTED_EDGE ( 'NONE', *, *, #4933, .F. ) ;
#3232 = CARTESIAN_POINT ( 'NONE',  ( -3.868085380944014329, 40.51689021754913256, 92.55433879953095300 ) ) ;
#3233 = CARTESIAN_POINT ( 'NONE',  ( 0.5920942507238189378, 52.36215724832370455, 76.86006382792197655 ) ) ;
#3234 = EDGE_LOOP ( 'NONE', ( #806, #11118, #3898, #19176, #9040 ) ) ;
#3235 = CARTESIAN_POINT ( 'NONE',  ( 2.741139475203663967, 48.81344869881760928, 95.05433879953095300 ) ) ;
#3236 = CARTESIAN_POINT ( 'NONE',  ( -4.477846259693498254, 36.96218137147968008, 53.35433879953099989 ) ) ;
#3237 = CARTESIAN_POINT ( 'NONE',  ( 0.6794293633488347472, 52.96080299881479192, 78.91894504275920497 ) ) ;
#3238 = CARTESIAN_POINT ( 'NONE',  ( -4.009385194876763592, 46.27527268018315709, 95.45433879611698558 ) ) ;
#3239 = CARTESIAN_POINT ( 'NONE',  ( 6.660594192354429843, 43.89417127335556046, 91.86058879782397923 ) ) ;
#3240 = EDGE_CURVE ( 'NONE', #10210, #4927, #16233, .T. ) ;
#3242 = EDGE_CURVE ( 'NONE', #6478, #12946, #16195, .T. ) ;
#3241 = LINE ( 'NONE', #19406, #19023 ) ;
#3243 = CARTESIAN_POINT ( 'NONE',  ( 4.454354847297358866, 39.79502961122975790, 90.11785626197793420 ) ) ;
#3244 = EDGE_CURVE ( 'NONE', #12818, #2386, #9338, .T. ) ;
#3245 = CARTESIAN_POINT ( 'NONE',  ( -3.495367959724249296, 36.18934821065389684, 76.68008248600652621 ) ) ;
#3246 = ORIENTED_EDGE ( 'NONE', *, *, #2074, .F. ) ;
#3247 = CARTESIAN_POINT ( 'NONE',  ( 1.859207995029386495, 52.95621058139879267, 79.18222496875146987 ) ) ;
#3248 = ORIENTED_EDGE ( 'NONE', *, *, #1836, .F. ) ;
#3249 = CARTESIAN_POINT ( 'NONE',  ( 5.220616844236031007, 45.87228208810806507, 92.79808879953097289 ) ) ;
#3250 = EDGE_CURVE ( 'NONE', #7497, #15145, #6321, .T. ) ;
#3251 = CARTESIAN_POINT ( 'NONE',  ( -7.600593896485820622, 45.28511094584521146, 75.45433879953088763 ) ) ;
#3252 = CARTESIAN_POINT ( 'NONE',  ( 9.177137044501376906, 42.29818641127601353, 79.38025142445083304 ) ) ;
#3253 = B_SPLINE_SURFACE_WITH_KNOTS ( 'NONE', 3, 1, ( 
 ( #12706, #15701 ),
 ( #1120, #2816 ),
 ( #10920, #9320 ),
 ( #15807, #3017 ),
 ( #9523, #6302 ),
 ( #12802, #19286 ),
 ( #4699, #17698 ),
 ( #3126, #8016 ),
 ( #6405, #12912 ),
 ( #3638, #5230 ),
 ( #16525, #4809 ) ),
 .UNSPECIFIED., .F., .F., .F.,
 ( 4, 1, 1, 1, 1, 1, 1, 1, 4 ),
 ( 2, 2 ),
 ( 0.000000000000000000, 0.2014779019512820402, 0.3683355476270177564, 0.4986267722911685296, 0.6014797591950403755, 0.6911751734036410966, 0.7846115128848750730, 0.8848135988872103397, 1.000000000000000000 ),
 ( 0.000000000000000000, 1.000000000000000000 ),
 .UNSPECIFIED. ) ;
#3254 = VERTEX_POINT ( 'NONE', #4719 ) ;
#3255 = FACE_OUTER_BOUND ( 'NONE', #11593, .T. ) ;
#3256 = CARTESIAN_POINT ( 'NONE',  ( -5.507966265829200125, 38.61198000306179523, 76.68644156968609593 ) ) ;
#3257 = ORIENTED_EDGE ( 'NONE', *, *, #2468, .T. ) ;
#3258 = CARTESIAN_POINT ( 'NONE',  ( 29.77115333998618496, 40.36218137147969287, 87.85433879953102121 ) ) ;
#3259 = CARTESIAN_POINT ( 'NONE',  ( 8.362247588757593775, 41.75942743809601865, 78.86713471249643703 ) ) ;
#3260 = CARTESIAN_POINT ( 'NONE',  ( -2.077846259693550746, 39.65884927180063357, 92.91433879953098085 ) ) ;
#3261 = ORIENTED_EDGE ( 'NONE', *, *, #14174, .T. ) ;
#3262 = CARTESIAN_POINT ( 'NONE',  ( -4.570740025688050601, 36.98368223715221603, 77.15538146413656762 ) ) ;
#3263 = CARTESIAN_POINT ( 'NONE',  ( -5.072433652944437377, 37.35426311015444867, 77.90218689189877921 ) ) ;
#3264 = CARTESIAN_POINT ( 'NONE',  ( 0.2541436421823717873, 38.02374091943176637, 91.54808879782400766 ) ) ;
#3265 = VERTEX_POINT ( 'NONE', #9749 ) ;
#3266 = CARTESIAN_POINT ( 'NONE',  ( -4.783040473602117260, 51.18705603930939674, 76.11505395997643575 ) ) ;
#3267 = PLANE ( 'NONE',  #13843 ) ;
#3268 = DIRECTION ( 'NONE',  ( 0.000000000000000000, 1.734723475976787846E-14, -1.000000000000000000 ) ) ;
#3269 = CARTESIAN_POINT ( 'NONE',  ( -4.536720638049474452, 37.70867145396312026, 76.33888740947983820 ) ) ;
#3270 = CARTESIAN_POINT ( 'NONE',  ( -4.158578283022523969, 37.42937009194850617, 78.34992703482498655 ) ) ;
#3271 = ADVANCED_FACE ( 'NONE', ( #13045 ), #11248, .T. ) ;
#3272 = FACE_OUTER_BOUND ( 'NONE', #10919, .T. ) ;
#3273 = CARTESIAN_POINT ( 'NONE',  ( 8.557023814081752278, 40.43966772045860125, 79.34450935619591405 ) ) ;
#3274 = ORIENTED_EDGE ( 'NONE', *, *, #18070, .T. ) ;
#3275 = CARTESIAN_POINT ( 'NONE',  ( -4.158578283022523081, 37.42937009194850617, 76.53375056423675460 ) ) ;
#3276 = CARTESIAN_POINT ( 'NONE',  ( 9.353817388681445522, 42.82770861117572281, 76.74257409364852833 ) ) ;
#3277 = EDGE_CURVE ( 'NONE', #11695, #7082, #3151, .T. ) ;
#3278 = CARTESIAN_POINT ( 'NONE',  ( 5.391786323697940198, 50.75965653268888644, 77.94845644658968808 ) ) ;
#3279 = CARTESIAN_POINT ( 'NONE',  ( 6.832223124813663340, 50.44160190723654580, 77.98033120372964788 ) ) ;
#3280 = EDGE_CURVE ( 'NONE', #2125, #4394, #5, .T. ) ;
#3281 = ORIENTED_EDGE ( 'NONE', *, *, #19722, .T. ) ;
#3282 = AXIS2_PLACEMENT_3D ( 'NONE', #8812, #16795, #18382 ) ;
#3283 = CYLINDRICAL_SURFACE ( 'NONE', #20922, 8.199999999999995737 ) ;
#3284 = CARTESIAN_POINT ( 'NONE',  ( -5.955451856753747109, 38.00651308716548726, 76.73301527011911105 ) ) ;
#3285 = DIRECTION ( 'NONE',  ( 0.7071067811865460184, 0.000000000000000000, 0.7071067811865490160 ) ) ;
#3286 = DIRECTION ( 'NONE',  ( -1.779391786395883536E-16, -5.922860397471806844E-17, 1.000000000000000000 ) ) ;
#3287 = CARTESIAN_POINT ( 'NONE',  ( 8.605722098886982252, 42.95003761989442381, 77.73063109826868811 ) ) ;
#3288 = CARTESIAN_POINT ( 'NONE',  ( -3.495065479208315562, 36.18912478048144266, 76.62933879953087057 ) ) ;
#3289 =( REPRESENTATION_RELATIONSHIP ('NONE','NONE', #11365, #14198 ) REPRESENTATION_RELATIONSHIP_WITH_TRANSFORMATION ( #12414 )SHAPE_REPRESENTATION_RELATIONSHIP( ) );
#3290 = CARTESIAN_POINT ( 'NONE',  ( 3.460444912181559474, 49.25145096859824889, 92.99246380123798872 ) ) ;
#3291 = ORIENTED_EDGE ( 'NONE', *, *, #16384, .F. ) ;
#3292 = CARTESIAN_POINT ( 'NONE',  ( -4.763142150953350473, 38.06180843274848513, 79.52089765539699329 ) ) ;
#3293 = CARTESIAN_POINT ( 'NONE',  ( 5.427780505986065762, 36.85179043424346190, 76.96022115247204454 ) ) ;
#3294 = CARTESIAN_POINT ( 'NONE',  ( 5.319138446618715044, 50.81266539351954492, 78.91899942818734814 ) ) ;
#3295 = CARTESIAN_POINT ( 'NONE',  ( -7.949137504989496783, 41.77948864320536160, 72.45433879953085921 ) ) ;
#3296 = CARTESIAN_POINT ( 'NONE',  ( 8.415472958870040543, 40.01543082757027747, 76.00709785348774972 ) ) ;
#3297 = ORIENTED_EDGE ( 'NONE', *, *, #3144, .F. ) ;
#3298 = VERTEX_POINT ( 'NONE', #15824 ) ;
#3299 = CARTESIAN_POINT ( 'NONE',  ( -0.2483056323647954422, 52.97321599846241469, 75.49651412033875886 ) ) ;
#3300 = VECTOR ( 'NONE', #16066, 1000.000000000000000 ) ;
#3301 = CARTESIAN_POINT ( 'NONE',  ( -0.1138099061810181750, 52.21093997964378985, 79.46489189366771200 ) ) ;
#3302 = CARTESIAN_POINT ( 'NONE',  ( 6.363981487871726905, 38.44054096167169376, 77.90902863000688683 ) ) ;
#3303 = CARTESIAN_POINT ( 'NONE',  ( -3.495392342740026415, 36.18936622140545012, 76.59109406773794149 ) ) ;
#3304 = CARTESIAN_POINT ( 'NONE',  ( 6.924055141134583202, 50.37376929599953712, 78.48669174070734300 ) ) ;
#3305 = ORIENTED_EDGE ( 'NONE', *, *, #20668, .T. ) ;
#3306 = CARTESIAN_POINT ( 'NONE',  ( 8.368699874006322759, 41.79530460399266900, 76.15680935856015310 ) ) ;
#3307 = ORIENTED_EDGE ( 'NONE', *, *, #7433, .T. ) ;
#3308 = CARTESIAN_POINT ( 'NONE',  ( 4.394343283833276992, 39.11584570990505938, 92.60183880123797451 ) ) ;
#3309 = VECTOR ( 'NONE', #14694, 999.9999999999998863 ) ;
#3310 = CARTESIAN_POINT ( 'NONE',  ( -6.613032277150674432, 45.52591812603678534, 79.45433879953087342 ) ) ;
#3311 = LINE ( 'NONE', #1411, #11368 ) ;
#3312 = EDGE_CURVE ( 'NONE', #10226, #9748, #3561, .T. ) ;
#3313 = CARTESIAN_POINT ( 'NONE',  ( 8.375221590814755146, 41.80223450334851520, 76.19888858912942453 ) ) ;
#3314 = AXIS2_PLACEMENT_3D ( 'NONE', #18629, #15549, #12457 ) ;
#3315 = CARTESIAN_POINT ( 'NONE',  ( 8.410029692550303082, 41.91954370998553969, 79.53253037310241780 ) ) ;
#3316 = ORIENTED_EDGE ( 'NONE', *, *, #19236, .T. ) ;
#3317 = CARTESIAN_POINT ( 'NONE',  ( 5.264787936635038967, 50.85164499159836282, 77.24089811989679788 ) ) ;
#3318 =( BOUNDED_CURVE ( )  B_SPLINE_CURVE ( 2, ( #6934, #237, #13439, #6726, #10048, #11847, #1948, #6832, #19911, #11959, #19811 ),
 .UNSPECIFIED., .F., .T. ) 
 B_SPLINE_CURVE_WITH_KNOTS ( ( 3, 2, 2, 2, 2, 3 ),
 ( 0.5173390146554853741, 0.5312500000000000000, 0.5625000000000000000, 0.5937500000000000000, 0.6250000000000000000, 0.6423390146554854852 ),
 .UNSPECIFIED. ) 
 CURVE ( )  GEOMETRIC_REPRESENTATION_ITEM ( )  RATIONAL_B_SPLINE_CURVE ( ( 0.9623977609649205789, 0.9661148573551010532, 1.000000000000000000, 0.9238795325112867385, 1.000000000000000000, 0.9238795325112867385, 1.000000000000000000, 0.9238795325112867385, 1.000000000000000000, 0.9577646751561854632, 0.9623977609649205789 ) ) 
 REPRESENTATION_ITEM ( '' )  );
#3319 = ORIENTED_EDGE ( 'NONE', *, *, #1990, .T. ) ;
#3320 = CARTESIAN_POINT ( 'NONE',  ( -7.702335971347676669, 47.29235430678204466, 78.19878669242514491 ) ) ;
#3321 = CARTESIAN_POINT ( 'NONE',  ( 6.828503391016846891, 43.33193468930419101, 90.41433880123798872 ) ) ;
#3322 = CARTESIAN_POINT ( 'NONE',  ( 2.043125170982144745, 38.48583871533720213, 93.77371380123798872 ) ) ;
#3323 = EDGE_LOOP ( 'NONE', ( #2799, #4202, #10900, #12902, #9815, #5671 ) ) ;
#3324 = CARTESIAN_POINT ( 'NONE',  ( 1.575197090673905009, 52.29457635664441284, 76.85862500479365167 ) ) ;
#3325 = PLANE ( 'NONE',  #4500 ) ;
#3326 = VECTOR ( 'NONE', #20857, 1000.000000000000000 ) ;
#3327 = CARTESIAN_POINT ( 'NONE',  ( 5.939862031672385356, 51.10075310024252815, 76.36217657474753651 ) ) ;
#3328 = CARTESIAN_POINT ( 'NONE',  ( -4.040577624441578308, 50.97067737579940427, 78.70491066849456274 ) ) ;
#3329 = CARTESIAN_POINT ( 'NONE',  ( 5.075432096899075596, 37.34693059362874834, 77.49967648550449439 ) ) ;
#3330 = EDGE_LOOP ( 'NONE', ( #18872, #11689, #16351, #18546 ) ) ;
#3331 = CARTESIAN_POINT ( 'NONE',  ( 31.22215374030650281, 42.76218137147968434, 78.80433879953099563 ) ) ;
#3332 = LINE ( 'NONE', #12808, #8958 ) ;
#3333 = ORIENTED_EDGE ( 'NONE', *, *, #17772, .F. ) ;
#3334 = PLANE ( 'NONE',  #6336 ) ;
#3335 = CARTESIAN_POINT ( 'NONE',  ( -7.620684125509877838, 40.70898352502287310, 77.18350490445806145 ) ) ;
#3336 = DIRECTION ( 'NONE',  ( -0.9485903129789527988, 0.3165065846431829311, -8.934458285744989980E-17 ) ) ;
#3337 = CARTESIAN_POINT ( 'NONE',  ( -1.590937568396969315, 39.63064243629642647, 93.26683879611698558 ) ) ;
#3338 = PLANE ( 'NONE',  #9669 ) ;
#3339 = DIRECTION ( 'NONE',  ( 0.5954989751681698529, -0.8033560671169786005, -5.234922652618076394E-17 ) ) ;
#3340 = CARTESIAN_POINT ( 'NONE',  ( 3.122075258343615545, 38.59543968120053847, 90.05576841395854615 ) ) ;
#3341 = CIRCLE ( 'NONE', #15245, 1.000000000000014655 ) ;
#3342 = CARTESIAN_POINT ( 'NONE',  ( 5.426594447001382271, 50.72524724735664847, 75.97375991483075097 ) ) ;
#3343 = EDGE_CURVE ( 'NONE', #16809, #10923, #10218, .T. ) ;
#3344 = ORIENTED_EDGE ( 'NONE', *, *, #3960, .F. ) ;
#3345 = CARTESIAN_POINT ( 'NONE',  ( 1.509564537322647615, 52.20629269272797757, 79.40139704896512285 ) ) ;
#3346 = LINE ( 'NONE', #14835, #3428 ) ;
#3347 = ORIENTED_EDGE ( 'NONE', *, *, #3170, .F. ) ;
#3348 = CARTESIAN_POINT ( 'NONE',  ( 23.03948732994508575, 36.35905713404685002, 76.90433879953101837 ) ) ;
#3349 = CARTESIAN_POINT ( 'NONE',  ( 10.77494014480653561, 42.96218137147968008, 73.80433879953100984 ) ) ;
#3350 = FACE_OUTER_BOUND ( 'NONE', #17389, .T. ) ;
#3351 = ORIENTED_EDGE ( 'NONE', *, *, #219, .F. ) ;
#3352 = DIRECTION ( 'NONE',  ( -0.3165065846431826535, -0.9485903129789529098, -2.188653791613874008E-16 ) ) ;
#3353 = CARTESIAN_POINT ( 'NONE',  ( -5.841826873769424111, 37.92258288932846710, 75.85972562479176418 ) ) ;
#3354 = ORIENTED_EDGE ( 'NONE', *, *, #1751, .T. ) ;
#3355 = CARTESIAN_POINT ( 'NONE',  ( 5.739147447831700610, 51.24901287804902239, 78.93590013629759028 ) ) ;
#3356 = DIRECTION ( 'NONE',  ( -1.540237394707284467E-16, -1.793354297423764243E-16, 1.000000000000000000 ) ) ;
#3357 = CARTESIAN_POINT ( 'NONE',  ( 3.948530577815480225, 39.69684013992245752, 94.39871379953098085 ) ) ;
#3358 = ORIENTED_EDGE ( 'NONE', *, *, #7772, .T. ) ;
#3359 = CARTESIAN_POINT ( 'NONE',  ( -4.603341302083757469, 37.00776348676620131, 77.20593245741272881 ) ) ;
#3360 = CARTESIAN_POINT ( 'NONE',  ( 24.43948732994508077, 45.16218137147969003, 76.90433879953101837 ) ) ;
#3361 = CARTESIAN_POINT ( 'NONE',  ( 4.673174852049363004, 39.63213674411673537, 91.70433879782397923 ) ) ;
#3362 = ORIENTED_EDGE ( 'NONE', *, *, #741, .T. ) ;
#3363 = CARTESIAN_POINT ( 'NONE',  ( -4.739054262994943478, 51.21848697497132719, 76.01646854312687651 ) ) ;
#3364 = CARTESIAN_POINT ( 'NONE',  ( 5.543189085303068531, 50.64520219118831079, 78.74294592654759128 ) ) ;
#3365 = CARTESIAN_POINT ( 'NONE',  ( 3.870209548259372578, 48.16803608786690205, 93.81846558602697428 ) ) ;
#3366 = CARTESIAN_POINT ( 'NONE',  ( -0.3080929418689875576, 37.85583172076933778, 93.69558880123800293 ) ) ;
#3367 = CARTESIAN_POINT ( 'NONE',  ( 8.850663652843866913, 41.31972494539268581, 77.52203278780699236 ) ) ;
#3368 = CARTESIAN_POINT ( 'NONE',  ( 4.381145549518540072, 37.02367899638166193, 75.57109918664292536 ) ) ;
#3369 = CIRCLE ( 'NONE', #9511, 5.199999999999999289 ) ;
#3370 = CARTESIAN_POINT ( 'NONE',  ( 7.675887208068574274, 40.16326346448608575, 77.75090705316073070 ) ) ;
#3371 = EDGE_LOOP ( 'NONE', ( #12774, #602, #12488, #6282, #1721, #15892, #11760, #9578, #3815, #9887, #1112, #8148, #838, #19267, #2102, #13880, #6079, #2205, #10620 ) ) ;
#3372 = FACE_BOUND ( 'NONE', #3487, .T. ) ;
#3373 = LINE ( 'NONE', #4860, #15014 ) ;
#3374 = CARTESIAN_POINT ( 'NONE',  ( -4.463792963332828378, 40.72925446781975722, 75.45433879953087342 ) ) ;
#3375 = CARTESIAN_POINT ( 'NONE',  ( 6.395410155697720533, 49.85024304639465953, 77.98033120372964788 ) ) ;
#3376 = VERTEX_POINT ( 'NONE', #1770 ) ;
#3377 = AXIS2_PLACEMENT_3D ( 'NONE', #10063, #5141, #11660 ) ;
#3378 = VECTOR ( 'NONE', #19540, 1000.000000000000000 ) ;
#3379 = CARTESIAN_POINT ( 'NONE',  ( 5.766510840975054286, 51.22880064179873472, 78.93606911575150775 ) ) ;
#3380 = VERTEX_POINT ( 'NONE', #13356 ) ;
#3381 = EDGE_CURVE ( 'NONE', #15424, #9111, #8251, .T. ) ;
#3382 = AXIS2_PLACEMENT_3D ( 'NONE', #11929, #10450, #3713 ) ;
#3383 = CARTESIAN_POINT ( 'NONE',  ( -2.802060903037110862, 47.69598914657549216, 79.04308574771191331 ) ) ;
#3385 = EDGE_CURVE ( 'NONE', #12858, #11872, #8676, .T. ) ;
#3384 =( NAMED_UNIT ( * ) SI_UNIT ( $, .STERADIAN. ) SOLID_ANGLE_UNIT ( ) );
#3386 = CARTESIAN_POINT ( 'NONE',  ( 2.091368541865485486, 52.21063245889818916, 72.45433879953087342 ) ) ;
#3387 = PLANE ( 'NONE',  #9952 ) ;
#3388 = CARTESIAN_POINT ( 'NONE',  ( -4.677846311233719412, 45.55551708285126722, 94.21487682030836197 ) ) ;
#3389 = CIRCLE ( 'NONE', #13935, 8.199999999999999289 ) ;
#3390 = CARTESIAN_POINT ( 'NONE',  ( 5.239500195294445994, 50.86496669987803187, 78.27515171461519117 ) ) ;
#3391 = AXIS2_PLACEMENT_3D ( 'NONE', #12421, #2730, #10738 ) ;
#3392 = DIRECTION ( 'NONE',  ( -0.5941461771851691553, -0.8043570849667760481, -2.357623395011396791E-16 ) ) ;
#3393 = CARTESIAN_POINT ( 'NONE',  ( 1.652727357819364418, 35.35299279957455099, 76.16022115247204738 ) ) ;
#3394 = CARTESIAN_POINT ( 'NONE',  ( -4.808920012916951592, 37.15961619924308934, 75.98775578934684916 ) ) ;
#3395 = EDGE_CURVE ( 'NONE', #5130, #9664, #5247, .T. ) ;
#3396 = AXIS2_PLACEMENT_3D ( 'NONE', #3331, #9836, #5022 ) ;
#3397 = CARTESIAN_POINT ( 'NONE',  ( 6.828503391016846891, 43.33193468930419101, 94.00808880123798872 ) ) ;
#3398 = ORIENTED_EDGE ( 'NONE', *, *, #1337, .T. ) ;
#3399 = CARTESIAN_POINT ( 'NONE',  ( 8.860816794629819526, 41.35015455542848173, 78.93613448519710118 ) ) ;
#3400 = EDGE_CURVE ( 'NONE', #19191, #4192, #18239, .T. ) ;
#3401 = DIRECTION ( 'NONE',  ( 1.402518428993831676E-16, -1.000000000000000000, 0.000000000000000000 ) ) ;
#3402 = CARTESIAN_POINT ( 'NONE',  ( -4.705149740856858998, 37.08296527939383935, 78.93669174070734584 ) ) ;
#3403 = CIRCLE ( 'NONE', #2394, 0.9921021478795020165 ) ;
#3404 = CARTESIAN_POINT ( 'NONE',  ( 8.293280423777593668, 41.56926772713645590, 77.52492703482499792 ) ) ;
#3405 = CARTESIAN_POINT ( 'NONE',  ( 28.52215374030649642, 40.36218137147969287, 87.65433879953101837 ) ) ;
#3406 = VERTEX_POINT ( 'NONE', #1968 ) ;
#3407 = EDGE_LOOP ( 'NONE', ( #3038, #4261, #7934, #18607 ) ) ;
#3409 = AXIS2_PLACEMENT_3D ( 'NONE', #18631, #15446, #18739 ) ;
#3408 = CARTESIAN_POINT ( 'NONE',  ( 6.379311811789950326, 38.45149544986467305, 75.97427057108799886 ) ) ;
#3410 = CARTESIAN_POINT ( 'NONE',  ( 4.639020460657009792, 52.06163236765677738, 78.92424046551381878 ) ) ;
#3411 = CARTESIAN_POINT ( 'NONE',  ( 6.445631799257238725, 38.49888528477907812, 77.41265765549051991 ) ) ;
#3412 = CARTESIAN_POINT ( 'NONE',  ( -3.607357127890973292, 36.27207009797979254, 75.89423958357750166 ) ) ;
#3413 = CARTESIAN_POINT ( 'NONE',  ( 5.515973886530674442, 50.66617152567425109, 78.02711337524276303 ) ) ;
#3414 = ORIENTED_EDGE ( 'NONE', *, *, #9033, .T. ) ;
#3415 =( REPRESENTATION_RELATIONSHIP ('NONE','NONE', #11365, #9056 ) REPRESENTATION_RELATIONSHIP_WITH_TRANSFORMATION ( #8909 )SHAPE_REPRESENTATION_RELATIONSHIP( ) );
#3416 = DIRECTION ( 'NONE',  ( -1.540237394707284220E-16, -1.793354297423764243E-16, 1.000000000000000000 ) ) ;
#3417 = ORIENTED_EDGE ( 'NONE', *, *, #1042, .T. ) ;
#3418 = CARTESIAN_POINT ( 'NONE',  ( -0.3080929418689875576, 37.85583172076933778, 92.44558880123798872 ) ) ;
#3419 = ADVANCED_FACE ( 'NONE', ( #10066 ), #15158, .F. ) ;
#3420 = CARTESIAN_POINT ( 'NONE',  ( 1.487944053602040295, 52.20654624397499788, 76.82903323957145858 ) ) ;
#3421 = CARTESIAN_POINT ( 'NONE',  ( 2.522153740306507075, 50.16218137147969713, 74.55433879953100984 ) ) ;
#3422 = CARTESIAN_POINT ( 'NONE',  ( 8.500816298777042590, 42.26161455596683680, 79.47732676628994852 ) ) ;
#3423 = ORIENTED_EDGE ( 'NONE', *, *, #12651, .F. ) ;
#3424 = LINE ( 'NONE', #11636, #9919 ) ;
#3425 = EDGE_LOOP ( 'NONE', ( #7049, #651, #13669, #18859, #13354, #11994, #5330, #9559, #20620, #16461, #17819, #13726 ) ) ;
#3426 = LINE ( 'NONE', #3736, #16658 ) ;
#3427 = CARTESIAN_POINT ( 'NONE',  ( 4.199109002476567376, 47.83913663364971569, 94.73786078214052964 ) ) ;
#3428 = VECTOR ( 'NONE', #8355, 1000.000000000000114 ) ;
#3429 = LINE ( 'NONE', #3634, #19664 ) ;
#3430 = ORIENTED_EDGE ( 'NONE', *, *, #2519, .T. ) ;
#3431 = LINE ( 'NONE', #2257, #7588 ) ;
#3432 = DIRECTION ( 'NONE',  ( -0.4999999999999977240, 0.8660254037844398178, -0.000000000000000000 ) ) ;
#3433 = CARTESIAN_POINT ( 'NONE',  ( 5.925645890915349767, 42.81779480767480095, 92.55433879953095300 ) ) ;
#3434 = CARTESIAN_POINT ( 'NONE',  ( 28.52215374030649642, 44.16218137147969003, 87.05433879953100984 ) ) ;
#3435 = CARTESIAN_POINT ( 'NONE',  ( 2.900946498003590612, 49.13729913812269245, 93.38297921192027218 ) ) ;
#3436 = ORIENTED_EDGE ( 'NONE', *, *, #9011, .F. ) ;
#3437 = B_SPLINE_CURVE_WITH_KNOTS ( 'NONE', 3,
 ( #16010, #12914, #3435, #16433, #4913, #6304 ),
 .UNSPECIFIED., .F., .F.,
 ( 4, 2, 4 ),
 ( 0.000000000000000000, 0.001381175314065562080, 0.002762350628131124159 ),
 .UNSPECIFIED. ) ;
#3438 = DIRECTION ( 'NONE',  ( -1.000000000000000000, 1.110223024625156540E-16, -1.779391786395883043E-16 ) ) ;
#3439 = CARTESIAN_POINT ( 'NONE',  ( 0.8453367053598014325, 52.35217735662078553, 78.54797669815580718 ) ) ;
#3440 = VERTEX_POINT ( 'NONE', #19925 ) ;
#3441 = CARTESIAN_POINT ( 'NONE',  ( 4.278870909452986204, 51.41364532819419964, 77.90619853385557292 ) ) ;
#3442 = DIRECTION ( 'NONE',  ( -1.402518428993831430E-16, 1.000000000000000000, -2.891205793294680792E-16 ) ) ;
#3443 = DIRECTION ( 'NONE',  ( -1.540237394707284467E-16, -1.793354297423764243E-16, 1.000000000000000000 ) ) ;
#3444 = CARTESIAN_POINT ( 'NONE',  ( -4.176309363623031068, 42.45208065485131499, 94.36058879611698558 ) ) ;
#3445 = VECTOR ( 'NONE', #19800, 1000.000000000000000 ) ;
#3446 = CARTESIAN_POINT ( 'NONE',  ( -4.007890887056452023, 40.01116025973682611, 93.89183879782397923 ) ) ;
#3447 = CARTESIAN_POINT ( 'NONE',  ( 5.486268716722809025, 37.64049940046611198, 76.11636564480957645 ) ) ;
#3448 = AXIS2_PLACEMENT_3D ( 'NONE', #1185, #10989, #4254 ) ;
#3449 =( BOUNDED_CURVE ( )  B_SPLINE_CURVE ( 2, ( #19524, #17080, #18780, #12300, #8683, #5578, #9000, #12082, #13876, #13558, #20470 ),
 .UNSPECIFIED., .F., .T. ) 
 B_SPLINE_CURVE_WITH_KNOTS ( ( 3, 2, 2, 2, 2, 3 ),
 ( 0.1769864399931200261, 0.1822857915258468686, 0.2083266188866827739, 0.2343674462475186793, 0.2604082736083545568, 0.2851266819498630145 ),
 .UNSPECIFIED. ) 
 CURVE ( )  GEOMETRIC_REPRESENTATION_ITEM ( )  RATIONAL_B_SPLINE_CURVE ( ( 0.9753234597474281786, 0.9845093586901592086, 1.000000000000000000, 0.9238795325112867385, 1.000000000000000000, 0.9238795325112867385, 1.000000000000000000, 0.9238795325112867385, 1.000000000000000000, 0.9277451222090459249, 0.9926614294311060238 ) ) 
 REPRESENTATION_ITEM ( '' )  );
#3450 = CARTESIAN_POINT ( 'NONE',  ( 5.599231707071657738, 51.35236299959863970, 78.30875056423674607 ) ) ;
#3451 = ORIENTED_EDGE ( 'NONE', *, *, #12458, .T. ) ;
#3452 = DIRECTION ( 'NONE',  ( -1.402518428993831676E-16, 1.000000000000000000, -0.000000000000000000 ) ) ;
#3453 = CYLINDRICAL_SURFACE ( 'NONE', #51, 8.199999999999995737 ) ;
#3454 = ADVANCED_FACE ( 'NONE', ( #18141 ), #2178, .F. ) ;
#3455 = EDGE_LOOP ( 'NONE', ( #5787, #20580, #7887, #11727 ) ) ;
#3456 = CARTESIAN_POINT ( 'NONE',  ( -1.534364324400819823, 49.45957383111225170, 93.44516862097951559 ) ) ;
#3457 = CARTESIAN_POINT ( 'NONE',  ( 3.816979860036839423, 48.22126577608943876, 92.57632317950277923 ) ) ;
#3458 = CARTESIAN_POINT ( 'NONE',  ( 8.299312890679575005, 42.03170978465910679, 75.38196330830126612 ) ) ;
#3459 = ORIENTED_EDGE ( 'NONE', *, *, #1313, .T. ) ;
#3460 = CARTESIAN_POINT ( 'NONE',  ( -5.784195910403845176, 44.99242805365518194, 96.03933880123796030 ) ) ;
#3461 = CARTESIAN_POINT ( 'NONE',  ( -4.972333685589229724, 38.21632979263497987, 75.48149882193594351 ) ) ;
#3462 = ORIENTED_EDGE ( 'NONE', *, *, #15634, .F. ) ;
#3463 = AXIS2_PLACEMENT_3D ( 'NONE', #13241, #18336, #3753 ) ;
#3464 = CARTESIAN_POINT ( 'NONE',  ( 5.599231707071657738, 51.35236299959863970, 78.59183879953087626 ) ) ;
#3465 = CARTESIAN_POINT ( 'NONE',  ( 0.9437382761187699254, 52.95236866523615760, 76.77576213461180998 ) ) ;
#3466 = CARTESIAN_POINT ( 'NONE',  ( 1.256812508749381774, 49.74246873332880625, 93.61746379953098085 ) ) ;
#3467 = AXIS2_PLACEMENT_3D ( 'NONE', #19140, #11067, #12545 ) ;
#3468 = VERTEX_POINT ( 'NONE', #8461 ) ;
#3469 = DIRECTION ( 'NONE',  ( 1.134288711164059445E-16, 1.000000000000000000, 7.183611964723549989E-17 ) ) ;
#3470 = CARTESIAN_POINT ( 'NONE',  ( -4.184856022532954078, 37.47340638715262173, 78.05402056118774112 ) ) ;
#3471 = EDGE_CURVE ( 'NONE', #15353, #16835, #19618, .T. ) ;
#3472 = ORIENTED_EDGE ( 'NONE', *, *, #5066, .F. ) ;
#3473 = CARTESIAN_POINT ( 'NONE',  ( -7.816538853785817587, 41.35010719132777979, 78.90520654368830833 ) ) ;
#3474 = DIRECTION ( 'NONE',  ( 3.893792155548169402E-16, 7.183611964723547524E-17, -1.000000000000000000 ) ) ;
#3475 = CARTESIAN_POINT ( 'NONE',  ( -1.077846259693481246, 47.82824192744437397, 69.55433879953100984 ) ) ;
#3476 = VECTOR ( 'NONE', #18077, 1000.000000000000000 ) ;
#3477 = DIRECTION ( 'NONE',  ( 2.838338907332122006E-16, -1.000000000000000000, 0.000000000000000000 ) ) ;
#3478 = CARTESIAN_POINT ( 'NONE',  ( 4.597212664172372953, 36.25829706351294135, 75.77524573853747825 ) ) ;
#3479 = AXIS2_PLACEMENT_3D ( 'NONE', #2991, #19574, #14267 ) ;
#3480 = CARTESIAN_POINT ( 'NONE',  ( 8.400787919062072007, 39.97141883166423781, 78.77723610448765612 ) ) ;
#3481 = ADVANCED_FACE ( 'NONE', ( #363, #7053, #16450 ), #6851, .T. ) ;
#3482 = ORIENTED_EDGE ( 'NONE', *, *, #13035, .F. ) ;
#3483 = CARTESIAN_POINT ( 'NONE',  ( -5.217375104949212528, 38.30559640794556486, 75.60320319432446468 ) ) ;
#3484 = CARTESIAN_POINT ( 'NONE',  ( 35.92215374030650565, 40.96218137147972982, 93.55433879953098142 ) ) ;
#3485 = DIRECTION ( 'NONE',  ( -0.5735764363510446051, -0.8191520442889927978, -0.000000000000000000 ) ) ;
#3486 = CARTESIAN_POINT ( 'NONE',  ( 2.119548831151183421, 52.81598568046361919, 78.26563523839334380 ) ) ;
#3487 = EDGE_LOOP ( 'NONE', ( #8598, #18899, #4210, #16635, #9824, #11739 ) ) ;
#3488 = VERTEX_POINT ( 'NONE', #17924 ) ;
#3489 = LINE ( 'NONE', #18173, #17111 ) ;
#3490 = VERTEX_POINT ( 'NONE', #10171 ) ;
#3491 = VECTOR ( 'NONE', #15005, 1000.000000000000000 ) ;
#3492 = ADVANCED_FACE ( 'NONE', ( #2073 ), #8569, .F. ) ;
#3493 = CARTESIAN_POINT ( 'NONE',  ( 7.726125090393122008, 40.24513420275368247, 76.01001584831250568 ) ) ;
#3494 = DIRECTION ( 'NONE',  ( 0.8146038580541355989, -0.5800177190770277047, 2.145060549590874096E-17 ) ) ;
#3495 = CARTESIAN_POINT ( 'NONE',  ( -0.07555581626192713063, 50.25084051303456789, 61.06567965797611919 ) ) ;
#3496 = DIRECTION ( 'NONE',  ( 1.000000000000000000, 0.000000000000000000, 0.000000000000000000 ) ) ;
#3497 = CARTESIAN_POINT ( 'NONE',  ( 5.052198367669454626, 48.31320248322255395, 93.26683879782399345 ) ) ;
#3498 = CARTESIAN_POINT ( 'NONE',  ( 5.611423337425062385, 41.22389019960463230, 93.92996380123805977 ) ) ;
#3499 = EDGE_CURVE ( 'NONE', #1377, #1091, #13453, .T. ) ;
#3500 = DIRECTION ( 'NONE',  ( 0.000000000000000000, 0.000000000000000000, -1.000000000000000000 ) ) ;
#3501 = LINE ( 'NONE', #8081, #11505 ) ;
#3502 = CARTESIAN_POINT ( 'NONE',  ( 5.611423337425062385, 41.22389019960463230, 93.92996380123798872 ) ) ;
#3503 = CARTESIAN_POINT ( 'NONE',  ( -0.3080929418689875576, 37.85583172076933778, 91.19558880123798872 ) ) ;
#3504 = ORIENTED_EDGE ( 'NONE', *, *, #2854, .T. ) ;
#3505 = EDGE_CURVE ( 'NONE', #2000, #13846, #9855, .T. ) ;
#3506 = CARTESIAN_POINT ( 'NONE',  ( 4.648737399797364667, 37.07553919738725057, 75.46805039548223704 ) ) ;
#3507 = EDGE_CURVE ( 'NONE', #12731, #1203, #1310, .T. ) ;
#3508 = ADVANCED_FACE ( 'NONE', ( #8357 ), #14838, .F. ) ;
#3509 = AXIS2_PLACEMENT_3D ( 'NONE', #400, #10996, #16579 ) ;
#3510 = CARTESIAN_POINT ( 'NONE',  ( 0.5221537403065112937, 44.16218137147969713, 46.35433879953098568 ) ) ;
#3511 = EDGE_CURVE ( 'NONE', #1769, #10226, #11976, .T. ) ;
#3512 = CARTESIAN_POINT ( 'NONE',  ( -4.886362818588788848, 37.21682008020638222, 78.74088963820604192 ) ) ;
#3513 = CARTESIAN_POINT ( 'NONE',  ( 8.951509595531131680, 41.62196663317372725, 77.18036020728871449 ) ) ;
#3514 = EDGE_CURVE ( 'NONE', #10923, #6568, #18453, .T. ) ;
#3515 = CARTESIAN_POINT ( 'NONE',  ( 9.201306621205869618, 42.37062416594873326, 78.02362291919803283 ) ) ;
#3516 = ORIENTED_EDGE ( 'NONE', *, *, #17661, .T. ) ;
#3517 = CARTESIAN_POINT ( 'NONE',  ( 4.591414450663933167, 52.09679700955160797, 78.70655549710109256 ) ) ;
#3518 = CARTESIAN_POINT ( 'NONE',  ( 6.880715602165139444, 37.89000465862396538, 77.41265765549051991 ) ) ;
#3519 = CARTESIAN_POINT ( 'NONE',  ( -3.716790732209381165, 36.35290429323533345, 75.71473766112499959 ) ) ;
#3520 = CARTESIAN_POINT ( 'NONE',  ( 0.8503282811412335995, 52.95606000782370870, 76.48963291717792856 ) ) ;
#3521 = ORIENTED_EDGE ( 'NONE', *, *, #17073, .F. ) ;
#3522 = DIRECTION ( 'NONE',  ( -0.5941461771851693774, -0.8043570849667760481, -2.357623395011396791E-16 ) ) ;
#3523 = VECTOR ( 'NONE', #20858, 1000.000000000000000 ) ;
#3524 = DIRECTION ( 'NONE',  ( -0.9485903129789527988, 0.3165065846431829311, -8.934458285744989980E-17 ) ) ;
#3525 = EDGE_LOOP ( 'NONE', ( #4754, #3946, #2844, #14312 ) ) ;
#3526 = CARTESIAN_POINT ( 'NONE',  ( -3.943187491250720544, 40.73580453397070755, 95.64871380294496817 ) ) ;
#3527 = CARTESIAN_POINT ( 'NONE',  ( 1.638828243247879790, 52.94402099307490772, 76.88486154722851040 ) ) ;
#3528 = CARTESIAN_POINT ( 'NONE',  ( 6.198496396448986090, 45.68315280215533392, 90.49246380123798872 ) ) ;
#3529 = B_SPLINE_CURVE_WITH_KNOTS ( 'NONE', 3,
 ( #11680, #3365, #19940, #19536, #1983, #1884 ),
 .UNSPECIFIED., .F., .F.,
 ( 4, 2, 4 ),
 ( 0.000000000000000000, 0.001391245437276853120, 0.002782490874553706240 ),
 .UNSPECIFIED. ) ;
#3530 = CARTESIAN_POINT ( 'NONE',  ( 8.648170029844118645, 43.06315486489794608, 78.41904468188381827 ) ) ;
#3531 = ORIENTED_EDGE ( 'NONE', *, *, #11507, .T. ) ;
#3532 = EDGE_CURVE ( 'NONE', #11879, #11628, #13870, .T. ) ;
#3533 = CARTESIAN_POINT ( 'NONE',  ( 1.365599874297942051, 40.36218137147969998, 46.22770477045764181 ) ) ;
#3534 = ORIENTED_EDGE ( 'NONE', *, *, #17686, .T. ) ;
#3535 = CARTESIAN_POINT ( 'NONE',  ( -1.306251101200017084, 49.87752504164859602, 69.32593395802447844 ) ) ;
#3536 = EDGE_CURVE ( 'NONE', #7189, #12515, #6452, .T. ) ;
#3537 = CARTESIAN_POINT ( 'NONE',  ( 4.454345183533989783, 39.79502090995749342, 90.27410581162071423 ) ) ;
#3538 = DIRECTION ( 'NONE',  ( -1.193617070626243484E-16, -1.000000000000000000, -0.000000000000000000 ) ) ;
#3539 = ORIENTED_EDGE ( 'NONE', *, *, #3868, .F. ) ;
#3540 = CARTESIAN_POINT ( 'NONE',  ( 24.32215374030650068, 44.16218137147968292, 87.05433879953099563 ) ) ;
#3541 = CARTESIAN_POINT ( 'NONE',  ( 1.514255888186003762, 51.36218137147968577, 83.03825919817350609 ) ) ;
#3542 = CARTESIAN_POINT ( 'NONE',  ( -3.495065479208315562, 36.18912478048144266, 76.62933879953087057 ) ) ;
#3543 = CARTESIAN_POINT ( 'NONE',  ( -4.032058992557826294, 50.97676447825651991, 78.59092584394873882 ) ) ;
#3544 = CARTESIAN_POINT ( 'NONE',  ( 0.5223315597379962760, 52.35472439729344529, 78.93427191990714675 ) ) ;
#3545 = ORIENTED_EDGE ( 'NONE', *, *, #11849, .T. ) ;
#3546 = CARTESIAN_POINT ( 'NONE',  ( -4.030157702633146322, 50.97812307042602953, 76.47051527011910821 ) ) ;
#3547 = VERTEX_POINT ( 'NONE', #16960 ) ;
#3548 = CARTESIAN_POINT ( 'NONE',  ( -3.098709854545130593, 36.80491647020841128, 78.46683879953087626 ) ) ;
#3549 = CARTESIAN_POINT ( 'NONE',  ( -6.743140149339597933, 40.41798080217650835, 77.97023824993468111 ) ) ;
#3550 = EDGE_CURVE ( 'NONE', #15252, #16139, #2699, .T. ) ;
#3551 = CARTESIAN_POINT ( 'NONE',  ( -4.158578283022522193, 37.42937009194850617, 76.81463291717793140 ) ) ;
#3552 = CARTESIAN_POINT ( 'NONE',  ( -1.187946976321871961, 48.86064447540922373, 92.79808879611698558 ) ) ;
#3553 = CARTESIAN_POINT ( 'NONE',  ( -4.209923912819721892, 38.70632820095286775, 77.33669174070733732 ) ) ;
#3554 = CARTESIAN_POINT ( 'NONE',  ( -1.419351766502867429, 49.49642391118513274, 92.25121379782397923 ) ) ;
#3555 = CARTESIAN_POINT ( 'NONE',  ( 5.807735516834878986, 37.12329237395520920, 76.04105433551922033 ) ) ;
#3556 = CARTESIAN_POINT ( 'NONE',  ( -6.910121556090746076, 47.56003565108909470, 78.32234914140835258 ) ) ;
#3557 = ORIENTED_EDGE ( 'NONE', *, *, #17672, .F. ) ;
#3558 = CARTESIAN_POINT ( 'NONE',  ( 8.722153740306486824, 36.96218137147968719, 95.05433879953098142 ) ) ;
#3559 = DIRECTION ( 'NONE',  ( -5.595882180570345180E-16, 1.000000000000000000, 0.000000000000000000 ) ) ;
#3560 = ORIENTED_EDGE ( 'NONE', *, *, #16758, .T. ) ;
#3561 = LINE ( 'NONE', #6640, #1716 ) ;
#3562 = CARTESIAN_POINT ( 'NONE',  ( 5.427780505986065762, 36.85179043424346190, 76.96022115247204454 ) ) ;
#3563 = CARTESIAN_POINT ( 'NONE',  ( 5.544968037009670780, 45.50804040601273925, 95.88308879953100927 ) ) ;
#3564 = VERTEX_POINT ( 'NONE', #2389 ) ;
#3565 = CARTESIAN_POINT ( 'NONE',  ( 3.357643116058062205, 50.56218137147968861, 92.03489701350649455 ) ) ;
#3566 = CARTESIAN_POINT ( 'NONE',  ( -5.921523028668194577, 37.98145122859525458, 76.14635491738357587 ) ) ;
#3567 = ORIENTED_EDGE ( 'NONE', *, *, #14800, .F. ) ;
#3568 = CARTESIAN_POINT ( 'NONE',  ( 2.522153740306510628, 49.81903562097208038, 53.15433879953100416 ) ) ;
#3569 = CARTESIAN_POINT ( 'NONE',  ( 0.4048777997643838167, 52.96142680216856746, 76.02501977270890166 ) ) ;
#3570 = CARTESIAN_POINT ( 'NONE',  ( -6.711723140599398896, 40.30068868319698083, 78.38758635656873253 ) ) ;
#3571 = EDGE_LOOP ( 'NONE', ( #20587, #18476, #4451, #20878 ) ) ;
#3572 = CARTESIAN_POINT ( 'NONE',  ( -4.547183694812711785, 37.74104324321675108, 77.90454030471208569 ) ) ;
#3573 = ORIENTED_EDGE ( 'NONE', *, *, #16514, .T. ) ;
#3574 = CARTESIAN_POINT ( 'NONE',  ( -4.239546901740170348, 50.82850121497202167, 75.97198585835440099 ) ) ;
#3575 = CARTESIAN_POINT ( 'NONE',  ( 5.316416202095706645, 37.50973464508803801, 75.36022115247205022 ) ) ;
#3576 =( BOUNDED_CURVE ( )  B_SPLINE_CURVE ( 2, ( #15756, #1172, #19040, #4452, #10972 ),
 .UNSPECIFIED., .F., .F. ) 
 B_SPLINE_CURVE_WITH_KNOTS ( ( 3, 2, 3 ),
 ( 0.3083811345117428160, 0.3250000000000000111, 0.3333811345117426717 ),
 .UNSPECIFIED. ) 
 CURVE ( )  GEOMETRIC_REPRESENTATION_ITEM ( )  RATIONAL_B_SPLINE_CURVE ( ( 0.9660722070828657859, 0.9493985675960727733, 1.000000000000000000, 0.9744809649152144093, 0.9660722070828662300 ) ) 
 REPRESENTATION_ITEM ( '' )  );
#3577 = DIRECTION ( 'NONE',  ( 0.000000000000000000, 0.000000000000000000, 1.000000000000000000 ) ) ;
#3578 = CARTESIAN_POINT ( 'NONE',  ( 6.203825325419909831, 49.98094110125470024, 75.61685692759286326 ) ) ;
#3579 = CARTESIAN_POINT ( 'NONE',  ( 0.3700437505152531781, 52.96086955526534013, 78.81268084498510973 ) ) ;
#3580 = CARTESIAN_POINT ( 'NONE',  ( 4.816229352426441679, 36.41479837022654920, 75.57109918664292536 ) ) ;
#3581 = CARTESIAN_POINT ( 'NONE',  ( 7.680169873459327334, 40.17609888434939336, 78.49952087821802138 ) ) ;
#3582 = ORIENTED_EDGE ( 'NONE', *, *, #15869, .T. ) ;
#3583 = CARTESIAN_POINT ( 'NONE',  ( 0.5221537403065019678, 44.16218137147968292, 72.45433879953087342 ) ) ;
#3584 = CARTESIAN_POINT ( 'NONE',  ( 8.354770124117221641, 42.19791863141301036, 75.41143022427675646 ) ) ;
#3585 = CARTESIAN_POINT ( 'NONE',  ( -1.202011496911927990, 49.96493122755408223, 72.45432679953087529 ) ) ;
#3586 = CARTESIAN_POINT ( 'NONE',  ( -5.784195910403845176, 44.99242805365518194, 94.78933880123798872 ) ) ;
#3587 = ORIENTED_EDGE ( 'NONE', *, *, #11328, .T. ) ;
#3588 = ORIENTED_EDGE ( 'NONE', *, *, #19324, .F. ) ;
#3589 = CARTESIAN_POINT ( 'NONE',  ( -2.500166695032102204, 48.49377146048119158, 94.97752763193327041 ) ) ;
#3590 = ORIENTED_EDGE ( 'NONE', *, *, #364, .T. ) ;
#3591 = CARTESIAN_POINT ( 'NONE',  ( -3.501255140781824426, 36.19369683415101946, 76.91456057462045237 ) ) ;
#3592 = LINE ( 'NONE', #14986, #5994 ) ;
#3593 = CARTESIAN_POINT ( 'NONE',  ( 4.286460013181947915, 51.39722162121891103, 77.51131257087278925 ) ) ;
#3594 = CARTESIAN_POINT ( 'NONE',  ( 0.4776854187739327795, 52.96289371955013081, 75.36214535001711567 ) ) ;
#3595 = EDGE_CURVE ( 'NONE', #15970, #557, #7602, .T. ) ;
#3596 = CARTESIAN_POINT ( 'NONE',  ( -3.628867371436364841, 48.69222599884265179, 94.82933879782399345 ) ) ;
#3597 = PRODUCT ( 'Main Case', 'Main Case', '', ( #13783 ) ) ;
#3598 = CARTESIAN_POINT ( 'NONE',  ( 0.6066065119434701502, 52.96541364096408699, 77.38437845781280089 ) ) ;
#3599 = CARTESIAN_POINT ( 'NONE',  ( 1.514255888186003984, 52.36218137147968577, 83.03825919817350609 ) ) ;
#3600 = CARTESIAN_POINT ( 'NONE',  ( 4.539819439306699955, 52.13490816606735478, 76.55090572632929025 ) ) ;
#3601 = CARTESIAN_POINT ( 'NONE',  ( 5.611423337425062385, 41.22389019960463230, 90.17996380123798872 ) ) ;
#3602 = CARTESIAN_POINT ( 'NONE',  ( -0.9988176903691428077, 49.83852402762217082, 90.64871380123798872 ) ) ;
#3603 = VERTEX_POINT ( 'NONE', #15379 ) ;
#3604 = CARTESIAN_POINT ( 'NONE',  ( 28.52215374030649642, 48.16218137147969003, 87.85433879953103542 ) ) ;
#3605 = EDGE_CURVE ( 'NONE', #8675, #13055, #15694, .T. ) ;
#3606 = CARTESIAN_POINT ( 'NONE',  ( -5.811565481342516826, 50.45210972548208161, 78.65111229433956908 ) ) ;
#3607 = CARTESIAN_POINT ( 'NONE',  ( 8.647902309851698277, 43.06067594696713030, 76.34338796316330900 ) ) ;
#3608 = CARTESIAN_POINT ( 'NONE',  ( 4.394343283833276992, 39.11584570990505938, 94.00808880123797451 ) ) ;
#3609 = CARTESIAN_POINT ( 'NONE',  ( -5.529385682154831727, 44.31555110708731604, 72.45433879953085921 ) ) ;
#3610 = LINE ( 'NONE', #3712, #778 ) ;
#3611 = ADVANCED_FACE ( 'NONE', ( #7379 ), #1113, .T. ) ;
#3612 = CARTESIAN_POINT ( 'NONE',  ( 2.722153740306499703, 47.73989013547934945, 50.15433879953098995 ) ) ;
#3613 = ORIENTED_EDGE ( 'NONE', *, *, #7724, .T. ) ;
#3614 = EDGE_LOOP ( 'NONE', ( #16476, #11946, #14823, #2072 ) ) ;
#3615 = DIRECTION ( 'NONE',  ( 1.540237394707284220E-16, 1.793354297423764243E-16, -1.000000000000000000 ) ) ;
#3616 = CARTESIAN_POINT ( 'NONE',  ( -3.580888326837074587, 36.25251866086962593, 75.96390267329995538 ) ) ;
#3617 = DIRECTION ( 'NONE',  ( -0.5941461771851727081, -0.8043570849667734945, -2.357623395011397284E-16 ) ) ;
#3618 = EDGE_LOOP ( 'NONE', ( #17612, #2292, #17204, #2712, #16419, #11428, #1030, #1138, #15911, #2708, #5101, #9805, #14390, #2922, #1232, #9621, #215, #17593, #3635, #8013, #19207, #16743, #17505, #6878, #10617, #143, #9563, #2300 ) ) ;
#3619 = EDGE_CURVE ( 'NONE', #6827, #5214, #13983, .T. ) ;
#3620 = CARTESIAN_POINT ( 'NONE',  ( -4.388990501910972952, 51.46862972198961472, 78.65149807507090429 ) ) ;
#3621 = AXIS2_PLACEMENT_3D ( 'NONE', #19655, #1808, #8288 ) ;
#3622 = LINE ( 'NONE', #10131, #2748 ) ;
#3623 = ORIENTED_EDGE ( 'NONE', *, *, #371, .T. ) ;
#3624 = CARTESIAN_POINT ( 'NONE',  ( -5.784195910403845176, 44.99242805365518194, 92.13308880123798872 ) ) ;
#3625 = CARTESIAN_POINT ( 'NONE',  ( 1.880005271900893948, 52.94211922356995359, 77.04052575557504667 ) ) ;
#3626 = EDGE_CURVE ( 'NONE', #14613, #17415, #4283, .T. ) ;
#3627 = CARTESIAN_POINT ( 'NONE',  ( 4.454354847297358866, 39.79502961122975790, 90.27410626197791998 ) ) ;
#3628 = LINE ( 'NONE', #13011, #8889 ) ;
#3629 = ORIENTED_EDGE ( 'NONE', *, *, #6765, .F. ) ;
#3630 = CARTESIAN_POINT ( 'NONE',  ( 8.872773925109784798, 41.38599083402314704, 79.54845644658969661 ) ) ;
#3631 = ORIENTED_EDGE ( 'NONE', *, *, #20629, .F. ) ;
#3632 = AXIS2_PLACEMENT_3D ( 'NONE', #19787, #1726, #13315 ) ;
#3633 = CARTESIAN_POINT ( 'NONE',  ( 6.282717385696039436, 38.32643750394947801, 79.45433879953087342 ) ) ;
#3634 = CARTESIAN_POINT ( 'NONE',  ( 2.115041367457930477, 52.20598078514409224, 72.45433879953087342 ) ) ;
#3635 = ORIENTED_EDGE ( 'NONE', *, *, #20158, .F. ) ;
#3636 = CARTESIAN_POINT ( 'NONE',  ( 0.5221537403065006355, 44.16218137147969003, 92.45433879953097289 ) ) ;
#3637 = CARTESIAN_POINT ( 'NONE',  ( -5.324466712459395623, 37.54042977870726361, 79.49842882144521639 ) ) ;
#3638 = CARTESIAN_POINT ( 'NONE',  ( -4.329272046085858250, 37.55995550954649786, 78.93589701864812014 ) ) ;
#3639 = CARTESIAN_POINT ( 'NONE',  ( 4.199109002476567376, 47.83913663364971569, 94.73786078214052964 ) ) ;
#3640 = DIRECTION ( 'NONE',  ( 1.540237394707284220E-16, 1.793354297423764243E-16, -1.000000000000000000 ) ) ;
#3641 = VERTEX_POINT ( 'NONE', #5790 ) ;
#3642 = ADVANCED_FACE ( 'NONE', ( #10716 ), #12397, .T. ) ;
#3643 = CARTESIAN_POINT ( 'NONE',  ( -4.388425821632080392, 51.46903322184264340, 76.24813767079230331 ) ) ;
#3644 = AXIS2_PLACEMENT_3D ( 'NONE', #1179, #1072, #17452 ) ;
#3645 = EDGE_LOOP ( 'NONE', ( #3663, #19723, #20216, #18662 ) ) ;
#3646 = CARTESIAN_POINT ( 'NONE',  ( -4.002097339596554448, 47.53156763023002895, 95.05433879953091036 ) ) ;
#3647 = EDGE_CURVE ( 'NONE', #14806, #7140, #14084, .T. ) ;
#3648 = CARTESIAN_POINT ( 'NONE',  ( -7.484136228611396824, 40.27717619252914716, 77.79645048995966761 ) ) ;
#3649 = CARTESIAN_POINT ( 'NONE',  ( -4.497956288874163100, 37.67830001658522576, 77.32061371610187450 ) ) ;
#3650 = CARTESIAN_POINT ( 'NONE',  ( -4.009385194876762704, 46.27527268018315709, 94.20433879611698558 ) ) ;
#3651 = CARTESIAN_POINT ( 'NONE',  ( 2.921181103050040306, 49.30691215337508737, 91.00121379782397923 ) ) ;
#3652 = DIRECTION ( 'NONE',  ( -0.9485903129789527988, 0.3165065846431829311, -8.934458285744989980E-17 ) ) ;
#3653 = ADVANCED_FACE ( 'NONE', ( #4190 ), #12592, .T. ) ;
#3654 = EDGE_CURVE ( 'NONE', #8370, #20845, #6295, .T. ) ;
#3655 = ORIENTED_EDGE ( 'NONE', *, *, #9722, .T. ) ;
#3656 = DIRECTION ( 'NONE',  ( -0.3165065846431827645, -0.9485903129789529098, 0.000000000000000000 ) ) ;
#3657 = EDGE_CURVE ( 'NONE', #17415, #468, #14604, .T. ) ;
#3658 = FACE_OUTER_BOUND ( 'NONE', #6026, .T. ) ;
#3659 = ORIENTED_EDGE ( 'NONE', *, *, #16750, .T. ) ;
#3660 = CARTESIAN_POINT ( 'NONE',  ( 10.77494014480653917, 42.96218137147968008, 61.40715055817103263 ) ) ;
#3661 = CARTESIAN_POINT ( 'NONE',  ( -2.077846259693550746, 39.65884927180063357, 96.66433879953098085 ) ) ;
#3662 = CARTESIAN_POINT ( 'NONE',  ( -4.500660556396669065, 42.81632233694663370, 96.50808879953099506 ) ) ;
#3663 = ORIENTED_EDGE ( 'NONE', *, *, #11832, .F. ) ;
#3664 = CARTESIAN_POINT ( 'NONE',  ( 9.026838159693451047, 41.84773111872319618, 78.13669174070733447 ) ) ;
#3665 = CARTESIAN_POINT ( 'NONE',  ( -5.157025508368715094, 37.41674770618860890, 75.39928922905468767 ) ) ;
#3666 = ORIENTED_EDGE ( 'NONE', *, *, #6710, .F. ) ;
#3667 = LINE ( 'NONE', #18042, #10151 ) ;
#3668 = CARTESIAN_POINT ( 'NONE',  ( 35.92215374030650565, 51.36218137147967866, 45.55433879953098852 ) ) ;
#3669 = VERTEX_POINT ( 'NONE', #4591 ) ;
#3670 = CARTESIAN_POINT ( 'NONE',  ( 0.5221537403065008576, 44.16218137147969003, 105.5543387995310098 ) ) ;
#3671 = CARTESIAN_POINT ( 'NONE',  ( 4.394343283833276992, 39.11584570990505938, 95.25808880123800293 ) ) ;
#3672 = VERTEX_POINT ( 'NONE', #20659 ) ;
#3673 = CARTESIAN_POINT ( 'NONE',  ( 0.6728307876203661886, 52.36082399497195894, 77.39742102862167883 ) ) ;
#3674 = LINE ( 'NONE', #8589, #1715 ) ;
#3675 = AXIS2_PLACEMENT_3D ( 'NONE', #19705, #6616, #1749 ) ;
#3676 =( NAMED_UNIT ( * ) PLANE_ANGLE_UNIT ( ) SI_UNIT ( $, .RADIAN. ) );
#3677 = ADVANCED_FACE ( 'NONE', ( #9724 ), #9516, .F. ) ;
#3678 = CARTESIAN_POINT ( 'NONE',  ( 2.635245049009968366, 48.69372030666295359, 94.20433879953097289 ) ) ;
#3679 = DIRECTION ( 'NONE',  ( -0.7071067811865535679, 1.203855704449247279E-16, -0.7071067811865414665 ) ) ;
#3680 = CARTESIAN_POINT ( 'NONE',  ( 4.029718316871106154, 36.77256196250399256, 76.05895398371444571 ) ) ;
#3681 = CARTESIAN_POINT ( 'NONE',  ( 7.786684689960352124, 40.49533054657691622, 79.21682452846883393 ) ) ;
#3682 = VERTEX_POINT ( 'NONE', #8010 ) ;
#3683 = DIRECTION ( 'NONE',  ( 0.000000000000000000, -1.000000000000000000, 0.000000000000000000 ) ) ;
#3684 = DIRECTION ( 'NONE',  ( -0.000000000000000000, -0.000000000000000000, -1.000000000000000000 ) ) ;
#3685 = CARTESIAN_POINT ( 'NONE',  ( -7.282021299424333627, 41.64493098333839072, 78.93502118727992922 ) ) ;
#3686 = ORIENTED_EDGE ( 'NONE', *, *, #10607, .T. ) ;
#3687 = ORIENTED_EDGE ( 'NONE', *, *, #18315, .T. ) ;
#3688 = CARTESIAN_POINT ( 'NONE',  ( 6.264934721967925668, 49.94661999341979453, 79.21482656134288902 ) ) ;
#3689 = ORIENTED_EDGE ( 'NONE', *, *, #268, .T. ) ;
#3690 = CARTESIAN_POINT ( 'NONE',  ( 30.43948732994509143, 45.16218137147969003, 76.90433879953101837 ) ) ;
#3691 = CARTESIAN_POINT ( 'NONE',  ( 8.648380609495486482, 40.71346983188059454, 75.44378286633819641 ) ) ;
#3692 = CARTESIAN_POINT ( 'NONE',  ( 1.855487073639850104, 49.49551470481303994, 61.82100546619766845 ) ) ;
#3693 = CARTESIAN_POINT ( 'NONE',  ( -7.376743071288318632, 41.96049357349896525, 78.50654468188380974 ) ) ;
#3694 = CARTESIAN_POINT ( 'NONE',  ( -5.368445182934982185, 36.96218137147968008, 93.55433879953098142 ) ) ;
#3695 = CARTESIAN_POINT ( 'NONE',  ( 2.122153740306496505, 47.82824192744437397, 69.55433879953100984 ) ) ;
#3696 = CARTESIAN_POINT ( 'NONE',  ( 0.7195706321513085646, 52.35316909177178246, 77.41791596341448667 ) ) ;
#3697 = DIRECTION ( 'NONE',  ( 0.000000000000000000, 0.000000000000000000, 1.000000000000000000 ) ) ;
#3698 = CARTESIAN_POINT ( 'NONE',  ( 4.110464395964859463, 51.52722249412126843, 76.26690125110441443 ) ) ;
#3699 = CARTESIAN_POINT ( 'NONE',  ( -0.3080929418689875576, 37.85583172076933778, 92.44558880123798872 ) ) ;
#3700 = AXIS2_PLACEMENT_3D ( 'NONE', #15846, #1582, #6455 ) ;
#3701 = DIRECTION ( 'NONE',  ( 0.9585804129707224952, 0.2848220354341972071, 1.987228219138359305E-16 ) ) ;
#3702 = CARTESIAN_POINT ( 'NONE',  ( 5.384092268968043271, 50.76532863195453160, 75.97198585835440099 ) ) ;
#3703 = AXIS2_PLACEMENT_3D ( 'NONE', #14553, #8165, #15947 ) ;
#3704 = VERTEX_POINT ( 'NONE', #1629 ) ;
#3705 = CARTESIAN_POINT ( 'NONE',  ( -4.546230963980875117, 36.96557838055436207, 76.09208750614521932 ) ) ;
#3706 = DIRECTION ( 'NONE',  ( -1.000000000000000000, 1.193617070626243484E-16, 0.000000000000000000 ) ) ;
#3707 = DIRECTION ( 'NONE',  ( 1.779391786395883536E-16, 5.922860397471806844E-17, -1.000000000000000000 ) ) ;
#3708 = CARTESIAN_POINT ( 'NONE',  ( 5.568489401881125289, 48.03437091500646261, 94.32058880123798872 ) ) ;
#3709 = EDGE_CURVE ( 'NONE', #5644, #14094, #3119, .T. ) ;
#3710 = AXIS2_PLACEMENT_3D ( 'NONE', #17285, #13776, #10820 ) ;
#3711 = LINE ( 'NONE', #2133, #1723 ) ;
#3712 = CARTESIAN_POINT ( 'NONE',  ( 6.282717385696040324, 38.32643750394948512, 72.45433879953087342 ) ) ;
#3713 = DIRECTION ( 'NONE',  ( 0.000000000000000000, 1.000000000000000000, 0.000000000000000000 ) ) ;
#3714 = ORIENTED_EDGE ( 'NONE', *, *, #14708, .F. ) ;
#3715 = ORIENTED_EDGE ( 'NONE', *, *, #14712, .T. ) ;
#3716 = AXIS2_PLACEMENT_3D ( 'NONE', #1687, #14349, #15951 ) ;
#3717 = CARTESIAN_POINT ( 'NONE',  ( 8.350753804761280819, 42.18588146751271495, 79.49775514261133935 ) ) ;
#3718 = CYLINDRICAL_SURFACE ( 'NONE', #16203, 4.199999999999999289 ) ;
#3719 = DIRECTION ( 'NONE',  ( -1.402518428993831676E-16, 1.000000000000000000, 0.000000000000000000 ) ) ;
#3720 = EDGE_LOOP ( 'NONE', ( #4159, #8568, #15375, #20223 ) ) ;
#3721 = CARTESIAN_POINT ( 'NONE',  ( 5.583914945631950566, 51.36367687427735973, 77.16202479023476712 ) ) ;
#3722 = EDGE_CURVE ( 'NONE', #8200, #15454, #8114, .T. ) ;
#3723 = DIRECTION ( 'NONE',  ( -1.402518428993831183E-16, 1.000000000000000000, -3.469446951953617640E-16 ) ) ;
#3725 = ADVANCED_FACE ( 'NONE', ( #20964 ), #12904, .F. ) ;
#3724 = CIRCLE ( 'NONE', #9185, 8.199999999999995737 ) ;
#3726 = CARTESIAN_POINT ( 'NONE',  ( 3.948530577815480225, 39.69684013992245752, 93.46121380294496817 ) ) ;
#3727 = CARTESIAN_POINT ( 'NONE',  ( -7.199302705971482474, 41.41278875884007959, 78.64066830726386570 ) ) ;
#3728 = CARTESIAN_POINT ( 'NONE',  ( 1.352400422481993658, 50.46853102219002096, 94.32058880123798872 ) ) ;
#3729 = VECTOR ( 'NONE', #16359, 1000.000000000000227 ) ;
#3730 = AXIS2_PLACEMENT_3D ( 'NONE', #13744, #765, #17048 ) ;
#3731 = LINE ( 'NONE', #864, #19741 ) ;
#3732 = EDGE_LOOP ( 'NONE', ( #13113, #6411, #20589, #12939 ) ) ;
#3733 = DIRECTION ( 'NONE',  ( 0.000000000000000000, 0.000000000000000000, 1.000000000000000000 ) ) ;
#3734 = VERTEX_POINT ( 'NONE', #10256 ) ;
#3735 = AXIS2_PLACEMENT_3D ( 'NONE', #9156, #17613, #3352 ) ;
#3736 = CARTESIAN_POINT ( 'NONE',  ( 2.337612517491833408, 49.93701999136722947, 75.45433879953087342 ) ) ;
#3737 = CARTESIAN_POINT ( 'NONE',  ( -4.524181921268124462, 40.28999182795290324, 91.03933880123798872 ) ) ;
#3738 = ORIENTED_EDGE ( 'NONE', *, *, #12768, .F. ) ;
#3739 = DIRECTION ( 'NONE',  ( -1.540237394707284220E-16, -1.793354297423764243E-16, 1.000000000000000000 ) ) ;
#3740 = FACE_OUTER_BOUND ( 'NONE', #1891, .T. ) ;
#3741 = CARTESIAN_POINT ( 'NONE',  ( 35.92215374030650565, 36.96218137147968719, 92.39963826115175038 ) ) ;
#3742 = ORIENTED_EDGE ( 'NONE', *, *, #20609, .F. ) ;
#3743 = AXIS2_PLACEMENT_3D ( 'NONE', #1986, #18364, #18054 ) ;
#3744 = CARTESIAN_POINT ( 'NONE',  ( -1.677846259693481112, 47.73989013547935656, 54.55433879953098852 ) ) ;
#3745 = EDGE_CURVE ( 'NONE', #6639, #15290, #20319, .T. ) ;
#3746 = ORIENTED_EDGE ( 'NONE', *, *, #4414, .F. ) ;
#3747 = CARTESIAN_POINT ( 'NONE',  ( -6.354755732003290802, 42.02918051195119631, 76.16022115247204738 ) ) ;
#3748 = CARTESIAN_POINT ( 'NONE',  ( -7.646773700855245437, 40.79148695562606264, 77.07900976289242578 ) ) ;
#3749 = CARTESIAN_POINT ( 'NONE',  ( 8.385679600361122255, 39.92613824206362949, 77.13595644658970230 ) ) ;
#3750 = CARTESIAN_POINT ( 'NONE',  ( 5.408052348349806415, 37.57667531233130376, 75.99391262232927602 ) ) ;
#3751 = VECTOR ( 'NONE', #13193, 1000.000000000000000 ) ;
#3752 = CARTESIAN_POINT ( 'NONE',  ( -1.876873622437038369, 39.01745058958429269, 91.62621379782397923 ) ) ;
#3753 = DIRECTION ( 'NONE',  ( -1.301042606982606060E-16, -1.000000000000000000, 0.000000000000000000 ) ) ;
#3754 = ORIENTED_EDGE ( 'NONE', *, *, #14500, .T. ) ;
#3755 = LINE ( 'NONE', #55, #9847 ) ;
#3756 = AXIS2_PLACEMENT_3D ( 'NONE', #1131, #12198, #18791 ) ;
#3757 = CARTESIAN_POINT ( 'NONE',  ( 0.5221537403065019678, 44.16218137147968292, 72.45433879953087342 ) ) ;
#3758 = EDGE_CURVE ( 'NONE', #15539, #16083, #16520, .T. ) ;
#3759 = EDGE_CURVE ( 'NONE', #11768, #13622, #9939, .T. ) ;
#3760 = ORIENTED_EDGE ( 'NONE', *, *, #3312, .F. ) ;
#3761 = DIRECTION ( 'NONE',  ( 0.000000000000000000, -1.000000000000000000, 0.000000000000000000 ) ) ;
#3762 = EDGE_CURVE ( 'NONE', #16089, #5649, #12725, .T. ) ;
#3763 = CARTESIAN_POINT ( 'NONE',  ( -4.500660556396669065, 42.81632233694663370, 94.00808879953098085 ) ) ;
#3764 = CARTESIAN_POINT ( 'NONE',  ( 4.987494971863720927, 47.58855820898865829, 93.46121379953098085 ) ) ;
#3765 = PRODUCT ( 'Locking Springs', 'Locking Springs', '', ( #4206 ) ) ;
#3766 = CARTESIAN_POINT ( 'NONE',  ( -7.435220081765090860, 42.57064376796103744, 76.77997794206987692 ) ) ;
#3767 = ORIENTED_EDGE ( 'NONE', *, *, #20265, .F. ) ;
#3768 = SURFACE_SIDE_STYLE ('',( #5468 ) ) ;
#3769 = DIRECTION ( 'NONE',  ( -0.000000000000000000, -0.000000000000000000, 1.000000000000000000 ) ) ;
#3770 = VERTEX_POINT ( 'NONE', #1743 ) ;
#3771 = CARTESIAN_POINT ( 'NONE',  ( -3.755573279388496832, 40.62988815434074752, 95.05433879953095300 ) ) ;
#3772 = CARTESIAN_POINT ( 'NONE',  ( -4.517072128342572768, 36.94403992325788977, 76.53375056423675460 ) ) ;
#3773 = ADVANCED_FACE ( 'NONE', ( #5118 ), #8431, .T. ) ;
#3774 = EDGE_CURVE ( 'NONE', #2822, #12006, #14697, .T. ) ;
#3775 = EDGE_LOOP ( 'NONE', ( #20646, #6854, #2483, #20438, #4129 ) ) ;
#3776 = CARTESIAN_POINT ( 'NONE',  ( -4.645483384943289273, 37.03889214578785527, 77.94562699264550076 ) ) ;
#3777 = CIRCLE ( 'NONE', #7178, 8.799999999999998934 ) ;
#3778 = ORIENTED_EDGE ( 'NONE', *, *, #8058, .T. ) ;
#3779 = CARTESIAN_POINT ( 'NONE',  ( -4.798777446476682584, 51.17581097466058537, 76.24916814194597237 ) ) ;
#3780 = DIRECTION ( 'NONE',  ( 1.000000000000000000, 0.000000000000000000, 0.000000000000000000 ) ) ;
#3781 = VECTOR ( 'NONE', #15426, 1000.000000000000000 ) ;
#3782 = EDGE_CURVE ( 'NONE', #19006, #4385, #336, .T. ) ;
#3783 = CARTESIAN_POINT ( 'NONE',  ( -4.357516591192297284, 37.58081861725695205, 75.97198585835440099 ) ) ;
#3784 = LINE ( 'NONE', #12001, #14954 ) ;
#3785 = CARTESIAN_POINT ( 'NONE',  ( 2.263811127080454622, 49.90383875825364157, 69.41268141275703840 ) ) ;
#3786 = ORIENTED_EDGE ( 'NONE', *, *, #10571, .T. ) ;
#3787 = ORIENTED_EDGE ( 'NONE', *, *, #5556, .F. ) ;
#3788 = DIRECTION ( 'NONE',  ( 1.540237394707284220E-16, 1.793354297423764243E-16, -1.000000000000000000 ) ) ;
#3789 = ORIENTED_EDGE ( 'NONE', *, *, #591, .F. ) ;
#3790 = AXIS2_PLACEMENT_3D ( 'NONE', #20522, #9267, #15757 ) ;
#3791 = DIRECTION ( 'NONE',  ( -3.942553354492745503E-16, 1.000000000000000000, 0.000000000000000000 ) ) ;
#3792 = CARTESIAN_POINT ( 'NONE',  ( 0.5706633979203369345, 52.96569706562746660, 77.38474949312757190 ) ) ;
#3793 = CARTESIAN_POINT ( 'NONE',  ( 1.352400422481993658, 50.46853102219002096, 95.72683880123798872 ) ) ;
#3794 = AXIS2_PLACEMENT_3D ( 'NONE', #8231, #11334, #17805 ) ;
#3795 = ORIENTED_EDGE ( 'NONE', *, *, #6981, .T. ) ;
#3796 = ORIENTED_EDGE ( 'NONE', *, *, #3762, .T. ) ;
#3797 = EDGE_CURVE ( 'NONE', #557, #10826, #5224, .T. ) ;
#3798 = CARTESIAN_POINT ( 'NONE',  ( 6.853523395152754105, 50.42586825556427499, 78.95155228521747404 ) ) ;
#3799 = ORIENTED_EDGE ( 'NONE', *, *, #13796, .F. ) ;
#3800 = CARTESIAN_POINT ( 'NONE',  ( 5.581238861929509909, 50.61552606843185487, 76.29031835629793079 ) ) ;
#3801 = CARTESIAN_POINT ( 'NONE',  ( 6.814395614697851933, 37.84261482370956031, 75.97427057108799886 ) ) ;
#3802 = CARTESIAN_POINT ( 'NONE',  ( 7.881290621023779863, 40.79563723267156661, 75.50010622114506020 ) ) ;
#3803 = DIRECTION ( 'NONE',  ( 1.000000000000000000, 0.000000000000000000, 0.000000000000000000 ) ) ;
#3804 = CYLINDRICAL_SURFACE ( 'NONE', #940, 6.200000000000000178 ) ;
#3805 = CARTESIAN_POINT ( 'NONE',  ( 8.314648285358305912, 41.60894804291065441, 77.52294762828243790 ) ) ;
#3806 = DIRECTION ( 'NONE',  ( -0.3165065846431824870, -0.9485903129789529098, 0.000000000000000000 ) ) ;
#3807 = CARTESIAN_POINT ( 'NONE',  ( 0.7243910816960694721, 52.96448486634505315, 77.41791596341448667 ) ) ;
#3809 = DIRECTION ( 'NONE',  ( 0.000000000000000000, 1.000000000000000000, -3.469446951953617147E-16 ) ) ;
#3808 = VECTOR ( 'NONE', #1257, 1000.000000000000000 ) ;
#3810 = CARTESIAN_POINT ( 'NONE',  ( 4.540684532156292086, 52.13426915682742901, 76.47586842453881673 ) ) ;
#3811 = CARTESIAN_POINT ( 'NONE',  ( 5.534247820986439415, 36.92786807952553119, 77.73906448345020692 ) ) ;
#3812 = CARTESIAN_POINT ( 'NONE',  ( 6.828503391016846891, 43.33193468930419101, 91.50808880123798872 ) ) ;
#3813 = VECTOR ( 'NONE', #17344, 1000.000000000000000 ) ;
#3814 = CARTESIAN_POINT ( 'NONE',  ( -7.953953629696516536, 41.76759382663043141, 78.67381781145438424 ) ) ;
#3815 = ORIENTED_EDGE ( 'NONE', *, *, #5529, .F. ) ;
#3816 = CARTESIAN_POINT ( 'NONE',  ( 4.185959258523188176, 36.82597263316856129, 75.77243029545449815 ) ) ;
#3817 = VERTEX_POINT ( 'NONE', #8221 ) ;
#3818 = DIRECTION ( 'NONE',  ( -1.000000000000000000, 9.340818716798192921E-14, 0.000000000000000000 ) ) ;
#3819 = DIRECTION ( 'NONE',  ( 1.000000000000000000, -0.000000000000000000, -0.000000000000000000 ) ) ;
#3820 = CARTESIAN_POINT ( 'NONE',  ( 8.318328750355229673, 41.62059619433301094, 75.36022115247205022 ) ) ;
#3821 = CARTESIAN_POINT ( 'NONE',  ( 4.613683346302097199, 40.84891852973634485, 90.69696562749766144 ) ) ;
#3822 = VECTOR ( 'NONE', #20090, 1000.000000000000000 ) ;
#3823 = FACE_OUTER_BOUND ( 'NONE', #17618, .T. ) ;
#3824 = DIRECTION ( 'NONE',  ( 1.540237394707284220E-16, 1.793354297423764243E-16, -1.000000000000000000 ) ) ;
#3825 = CARTESIAN_POINT ( 'NONE',  ( 5.819883890974968388, 51.18937611976139834, 77.96367690144739981 ) ) ;
#3826 = EDGE_LOOP ( 'NONE', ( #9500, #10712, #11359, #17078 ) ) ;
#3827 = EDGE_LOOP ( 'NONE', ( #11575, #2190, #19726, #14940 ) ) ;
#3828 = CARTESIAN_POINT ( 'NONE',  ( 31.03948732994507864, 43.16218137147969003, 78.30433879953099563 ) ) ;
#3829 = LINE ( 'NONE', #10350, #18262 ) ;
#3830 = CARTESIAN_POINT ( 'NONE',  ( 6.813511439209503529, 39.88797755036236481, 72.45432679953087529 ) ) ;
#3831 = ORIENTED_EDGE ( 'NONE', *, *, #1579, .F. ) ;
#3832 = DIRECTION ( 'NONE',  ( -1.110223024625156540E-16, -1.000000000000000000, -5.922860397471808077E-17 ) ) ;
#3833 = DIRECTION ( 'NONE',  ( 0.8043570849667760481, -0.5941461771851693774, 1.733862608106482338E-17 ) ) ;
#3834 = DIRECTION ( 'NONE',  ( -3.893792155548169402E-16, -7.183611964723547524E-17, 1.000000000000000000 ) ) ;
#3835 = CARTESIAN_POINT ( 'NONE',  ( 4.987494971863720927, 47.58855820898865829, 92.52371380294498238 ) ) ;
#3836 = EDGE_CURVE ( 'NONE', #3641, #3770, #14256, .T. ) ;
#3837 = CARTESIAN_POINT ( 'NONE',  ( 1.493768332708312441, 52.94516484377990651, 76.82903323957145858 ) ) ;
#3838 = VECTOR ( 'NONE', #15780, 1000.000000000000000 ) ;
#3839 = CARTESIAN_POINT ( 'NONE',  ( 4.394343283833276992, 39.11584570990505938, 93.85183880123797451 ) ) ;
#3840 = LINE ( 'NONE', #10362, #5820 ) ;
#3841 = VERTEX_POINT ( 'NONE', #3633 ) ;
#3842 = CARTESIAN_POINT ( 'NONE',  ( 8.303614452336031349, 41.57589654819728509, 79.54845644658969661 ) ) ;
#3843 = ORIENTED_EDGE ( 'NONE', *, *, #19899, .T. ) ;
#3844 = CARTESIAN_POINT ( 'NONE',  ( -4.785381074711875016, 51.18538353145122954, 78.79723525346945223 ) ) ;
#3845 = CARTESIAN_POINT ( 'NONE',  ( -0.9988176903691428077, 49.83852402762217082, 93.14871380123798872 ) ) ;
#3846 = EDGE_LOOP ( 'NONE', ( #605, #9938, #3521, #6606 ) ) ;
#3847 = CARTESIAN_POINT ( 'NONE',  ( -5.478128554961354091, 38.57320898139802523, 72.45433879953085921 ) ) ;
#3848 = VECTOR ( 'NONE', #18676, 1000.000000000000227 ) ;
#3849 = DIRECTION ( 'NONE',  ( -0.5670994908670430323, 0.8236492988270800453, 6.036271672687320902E-17 ) ) ;
#3850 = CARTESIAN_POINT ( 'NONE',  ( 8.200913038183980319, 41.32723632482947806, 77.80727997600146750 ) ) ;
#3851 = CARTESIAN_POINT ( 'NONE',  ( 0.7565349869329739407, 52.95907566945976441, 77.43632499672374081 ) ) ;
#3852 = CARTESIAN_POINT ( 'NONE',  ( 0.8503874818422292314, 52.96356767324962078, 76.48963291717792856 ) ) ;
#3853 = CARTESIAN_POINT ( 'NONE',  ( 0.3279640439667346752, 52.35988168082470651, 77.10139762306027933 ) ) ;
#3854 = EDGE_LOOP ( 'NONE', ( #12920, #87, #6116, #11038 ) ) ;
#3855 = PLANE ( 'NONE',  #12255 ) ;
#3856 = VERTEX_POINT ( 'NONE', #19489 ) ;
#3857 = CARTESIAN_POINT ( 'NONE',  ( -4.498303996637021740, 46.81144376258747997, 95.05433879953096721 ) ) ;
#3858 = DIRECTION ( 'NONE',  ( 0.000000000000000000, 1.734723475976787531E-14, -1.000000000000000000 ) ) ;
#3859 = EDGE_CURVE ( 'NONE', #10995, #14152, #10144, .T. ) ;
#3860 = CARTESIAN_POINT ( 'NONE',  ( 6.152864644243832615, 50.94341665060460400, 79.51305506302354331 ) ) ;
#3861 = CARTESIAN_POINT ( 'NONE',  ( -1.419351766502868761, 49.49642391118513274, 94.75121379782397923 ) ) ;
#3862 = CARTESIAN_POINT ( 'NONE',  ( 5.848563030374239524, 37.15246622033975399, 76.55482881315118959 ) ) ;
#3863 = AXIS2_PLACEMENT_3D ( 'NONE', #11037, #19517, #4929 ) ;
#3864 = ORIENTED_EDGE ( 'NONE', *, *, #15312, .T. ) ;
#3865 = CARTESIAN_POINT ( 'NONE',  ( 4.394187631985148279, 51.39056414810583817, 77.57533925735273783 ) ) ;
#3866 = VERTEX_POINT ( 'NONE', #8542 ) ;
#3867 = DIRECTION ( 'NONE',  ( 0.8043570849667761591, -0.5941461771851690443, 1.733862608106491891E-17 ) ) ;
#3868 = EDGE_CURVE ( 'NONE', #4394, #18879, #18006, .T. ) ;
#3869 = CARTESIAN_POINT ( 'NONE',  ( 1.256812508749381774, 49.74246873332880625, 94.86746379953099506 ) ) ;
#3870 = CARTESIAN_POINT ( 'NONE',  ( 4.987494971863720927, 47.58855820898865829, 94.71121379953099506 ) ) ;
#3871 = VERTEX_POINT ( 'NONE', #6928 ) ;
#3872 = DIRECTION ( 'NONE',  ( -5.626130192357176673E-16, -1.831515347669941892E-30, 1.000000000000000000 ) ) ;
#3873 = DIRECTION ( 'NONE',  ( -3.211742425186504723E-16, 5.922860397471811774E-17, -1.000000000000000000 ) ) ;
#3874 = ORIENTED_EDGE ( 'NONE', *, *, #17712, .F. ) ;
#3875 = CARTESIAN_POINT ( 'NONE',  ( 0.3607607205289448116, 38.91027021862021940, 95.05433879953098142 ) ) ;
#3876 = CARTESIAN_POINT ( 'NONE',  ( -4.799400614414246036, 51.17536568166803335, 78.65631888207801126 ) ) ;
#3877 = ORIENTED_EDGE ( 'NONE', *, *, #3400, .T. ) ;
#3878 = FACE_OUTER_BOUND ( 'NONE', #16014, .T. ) ;
#3879 = CARTESIAN_POINT ( 'NONE',  ( -4.567115856812060670, 47.10047254335474065, 94.71121380123797451 ) ) ;
#3880 = ORIENTED_EDGE ( 'NONE', *, *, #11484, .T. ) ;
#3881 = CARTESIAN_POINT ( 'NONE',  ( -4.451201164328465687, 50.67726082808356836, 76.41659450085566618 ) ) ;
#3882 = FACE_OUTER_BOUND ( 'NONE', #7075, .T. ) ;
#3883 = EDGE_CURVE ( 'NONE', #12307, #4579, #3426, .T. ) ;
#3884 = ADVANCED_FACE ( 'NONE', ( #17898, #18636 ), #8967, .T. ) ;
#3885 = CARTESIAN_POINT ( 'NONE',  ( 5.568489401881125289, 48.03437091500646261, 90.41433880123798872 ) ) ;
#3886 = EDGE_CURVE ( 'NONE', #5474, #8207, #12372, .T. ) ;
#3887 = CARTESIAN_POINT ( 'NONE',  ( -3.584565806390782594, 36.25523506687804343, 78.05869123030269918 ) ) ;
#3888 = DIRECTION ( 'NONE',  ( 1.540237394707284220E-16, 1.793354297423764243E-16, -1.000000000000000000 ) ) ;
#3889 = EDGE_CURVE ( 'NONE', #7228, #11865, #9311, .T. ) ;
#3890 = ORIENTED_EDGE ( 'NONE', *, *, #6992, .F. ) ;
#3891 = ORIENTED_EDGE ( 'NONE', *, *, #12338, .F. ) ;
#3892 = ADVANCED_FACE ( 'NONE', ( #16935 ), #5955, .T. ) ;
#3893 = CARTESIAN_POINT ( 'NONE',  ( 1.966680432375413012, 52.20268719857811135, 75.87378281519762879 ) ) ;
#3894 = ORIENTED_EDGE ( 'NONE', *, *, #11826, .F. ) ;
#3895 = DIRECTION ( 'NONE',  ( -0.9485903129789527988, 0.3165065846431829311, -8.934458285744989980E-17 ) ) ;
#3896 = FACE_OUTER_BOUND ( 'NONE', #16141, .T. ) ;
#3897 = CARTESIAN_POINT ( 'NONE',  ( -3.350035803220276609, 49.20851703305431357, 95.88308880123798872 ) ) ;
#3898 = ORIENTED_EDGE ( 'NONE', *, *, #7248, .F. ) ;
#3899 = DIRECTION ( 'NONE',  ( -0.5941461771851691553, -0.8043570849667760481, -2.357623395011396791E-16 ) ) ;
#3900 = VERTEX_POINT ( 'NONE', #4164 ) ;
#3901 = DIRECTION ( 'NONE',  ( 0.9485903129789495791, -0.3165065846431930341, 8.934458285744763183E-17 ) ) ;
#3902 = DIRECTION ( 'NONE',  ( -0.3165065846431828200, -0.9485903129789529098, 0.000000000000000000 ) ) ;
#3903 = B_SPLINE_CURVE_WITH_KNOTS ( 'NONE', 3,
 ( #1375, #1482, #11169, #14453, #20919, #6354, #12855, #19444, #11277, #3182, #17439, #9684 ),
 .UNSPECIFIED., .F., .F.,
 ( 4, 2, 2, 2, 2, 4 ),
 ( 4.336808689942017736E-19, 0.0001693000378404274555, 0.0003386000756808544773, 0.0004232500946010679882, 0.0005079001135212814991, 0.0006772001513616680802 ),
 .UNSPECIFIED. ) ;
#3904 = CARTESIAN_POINT ( 'NONE',  ( -1.477846259693484265, 49.81903562097206617, 123.5543387995310098 ) ) ;
#3905 = CARTESIAN_POINT ( 'NONE',  ( -2.917199766949190476, 51.60602765227618960, 78.10580938776615767 ) ) ;
#3906 = DIRECTION ( 'NONE',  ( -0.000000000000000000, 1.000000000000000000, -0.000000000000000000 ) ) ;
#3907 = CARTESIAN_POINT ( 'NONE',  ( 11.22215374030649926, 42.96218137147968008, 77.40433879953098995 ) ) ;
#3908 = CARTESIAN_POINT ( 'NONE',  ( 8.218197382629700343, 41.34423908963691474, 76.14505377247542128 ) ) ;
#3909 = CARTESIAN_POINT ( 'NONE',  ( -0.08603609158598878037, 38.30449681981696841, 92.55433879953098142 ) ) ;
#3910 = DIRECTION ( 'NONE',  ( -1.540237394707283727E-16, -1.793354297423763257E-16, 1.000000000000000000 ) ) ;
#3911 = ADVANCED_FACE ( 'NONE', ( #10687 ), #15350, .F. ) ;
#3912 = CARTESIAN_POINT ( 'NONE',  ( -2.904223097202481174, 48.62752260303690122, 92.83621380294498238 ) ) ;
#3913 = CARTESIAN_POINT ( 'NONE',  ( 8.373001147486398565, 41.79479491692730164, 76.15241572602435838 ) ) ;
#3914 = ORIENTED_EDGE ( 'NONE', *, *, #2067, .F. ) ;
#3915 = EDGE_CURVE ( 'NONE', #6086, #19935, #5550, .T. ) ;
#3916 = CARTESIAN_POINT ( 'NONE',  ( -7.333990156426534845, 40.19720935722482835, 72.45433879953085921 ) ) ;
#3917 = EDGE_CURVE ( 'NONE', #5383, #10416, #7463, .T. ) ;
#3918 = ORIENTED_EDGE ( 'NONE', *, *, #13471, .T. ) ;
#3919 = CARTESIAN_POINT ( 'NONE',  ( 8.789147962602239517, 47.20595287382010241, 75.43669174070734584 ) ) ;
#3920 = DIRECTION ( 'NONE',  ( -0.3165065846431827645, -0.9485903129789529098, 0.000000000000000000 ) ) ;
#3921 = CARTESIAN_POINT ( 'NONE',  ( -4.337246640924047547, 50.76736814398887532, 78.93151080536149777 ) ) ;
#3922 = CARTESIAN_POINT ( 'NONE',  ( -4.524181921268124462, 40.28999182795290324, 96.19558880123798872 ) ) ;
#3923 = DIRECTION ( 'NONE',  ( -0.3165065846431826535, -0.9485903129789529098, -2.188653791613874008E-16 ) ) ;
#3924 = DIRECTION ( 'NONE',  ( 1.540237394707284220E-16, 1.793354297423764243E-16, -1.000000000000000000 ) ) ;
#3925 = DIRECTION ( 'NONE',  ( -1.540237394707284467E-16, -1.793354297423764243E-16, 1.000000000000000000 ) ) ;
#3926 = LINE ( 'NONE', #10121, #9172 ) ;
#3927 = VERTEX_POINT ( 'NONE', #18847 ) ;
#3928 = VERTEX_POINT ( 'NONE', #15136 ) ;
#3929 = CARTESIAN_POINT ( 'NONE',  ( 6.153536035488349043, 50.12267912296926653, 77.68963291717793140 ) ) ;
#3930 = CARTESIAN_POINT ( 'NONE',  ( 8.832380548758539618, 43.45507459029313679, 73.00433879953099847 ) ) ;
#3931 = CARTESIAN_POINT ( 'NONE',  ( 8.951454296033540814, 41.62180089707131003, 76.31823237213514233 ) ) ;
#3932 = VERTEX_POINT ( 'NONE', #546 ) ;
#3933 = CARTESIAN_POINT ( 'NONE',  ( 0.5221537403065191763, 44.16218137147969003, 53.55433879953099563 ) ) ;
#3934 = CARTESIAN_POINT ( 'NONE',  ( 5.633915549615357676, 51.32674344226200702, 77.24912405724838038 ) ) ;
#3935 = CARTESIAN_POINT ( 'NONE',  ( -4.526015856129116166, 36.95064629469848683, 78.75608284215286403 ) ) ;
#3936 = CARTESIAN_POINT ( 'NONE',  ( -2.077846259693550746, 39.65884927180063357, 91.97683880294496817 ) ) ;
#3937 = CARTESIAN_POINT ( 'NONE',  ( -0.7639737096562715379, 52.86806976190393215, 79.04649434735723901 ) ) ;
#3938 = CARTESIAN_POINT ( 'NONE',  ( -3.554968601118880134, 36.23337280359183410, 78.17158301229430606 ) ) ;
#3939 = CARTESIAN_POINT ( 'NONE',  ( -7.622107932457680590, 47.55268842043668087, 78.30768265673681583 ) ) ;
#3940 = ADVANCED_FACE ( 'NONE', ( #7028 ), #10366, .F. ) ;
#3941 = CARTESIAN_POINT ( 'NONE',  ( 2.043125170982144745, 38.48583871533720213, 93.77371380123798872 ) ) ;
#3942 = PRODUCT_DEFINITION_SHAPE ( 'NONE', 'NONE',  #385 ) ;
#3943 = DIRECTION ( 'NONE',  ( -1.779391786395883536E-16, -5.922860397471806844E-17, 1.000000000000000000 ) ) ;
#3944 = ORIENTED_EDGE ( 'NONE', *, *, #12353, .T. ) ;
#3945 = CARTESIAN_POINT ( 'NONE',  ( 5.839579929017896021, 51.17482744986389775, 77.27318761637275202 ) ) ;
#3946 = ORIENTED_EDGE ( 'NONE', *, *, #15853, .T. ) ;
#3947 = CARTESIAN_POINT ( 'NONE',  ( -4.705661087595403025, 51.24234851550965431, 78.91934866582661812 ) ) ;
#3948 = CARTESIAN_POINT ( 'NONE',  ( -0.2125050281363792815, 38.58189400963055959, 94.55496380294496817 ) ) ;
#3949 = ORIENTED_EDGE ( 'NONE', *, *, #7658, .T. ) ;
#3950 = CARTESIAN_POINT ( 'NONE',  ( -3.628867371436363953, 48.69222599884265179, 93.73558879782399345 ) ) ;
#3951 = CARTESIAN_POINT ( 'NONE',  ( 0.5221537403065040772, 39.16218137147969003, 94.91636871766883132 ) ) ;
#3952 = CIRCLE ( 'NONE', #5295, 3.999999999999996447 ) ;
#3953 = CARTESIAN_POINT ( 'NONE',  ( -3.415291652819150592, 51.24462368788206845, 79.38294305353919356 ) ) ;
#3954 = LINE ( 'NONE', #15357, #17249 ) ;
#3955 = CARTESIAN_POINT ( 'NONE',  ( 5.427780505986065762, 36.85179043424346190, 76.96022115247204454 ) ) ;
#3956 = CARTESIAN_POINT ( 'NONE',  ( 0.3400554298508484674, 52.96751499973433397, 78.67509294885779525 ) ) ;
#3957 = EDGE_LOOP ( 'NONE', ( #17378, #10605, #2703, #18252 ) ) ;
#3958 = CARTESIAN_POINT ( 'NONE',  ( 8.644901377098815232, 43.03925179711409754, 72.45433879953087342 ) ) ;
#3959 = VERTEX_POINT ( 'NONE', #5967 ) ;
#3960 = EDGE_CURVE ( 'NONE', #14953, #20498, #3403, .T. ) ;
#3961 = LINE ( 'NONE', #16950, #14851 ) ;
#3962 = FACE_OUTER_BOUND ( 'NONE', #11065, .T. ) ;
#3963 = CARTESIAN_POINT ( 'NONE',  ( 5.496261972130637830, 37.64311312718927383, 76.46034384425426822 ) ) ;
#3964 = CARTESIAN_POINT ( 'NONE',  ( -1.876873622437039701, 39.01745058958429269, 94.12621379782397923 ) ) ;
#3965 = CARTESIAN_POINT ( 'NONE',  ( -5.419656513257913311, 37.61074265007807327, 75.48149882193594351 ) ) ;
#3966 = CIRCLE ( 'NONE', #8742, 8.799999999999995381 ) ;
#3967 = CARTESIAN_POINT ( 'NONE',  ( 5.500237024828340537, 36.90356520980568433, 77.71779572520892998 ) ) ;
#3968 = ORIENTED_EDGE ( 'NONE', *, *, #13386, .F. ) ;
#3969 = ORIENTED_EDGE ( 'NONE', *, *, #16127, .T. ) ;
#3970 = CARTESIAN_POINT ( 'NONE',  ( -3.722637431614235659, 51.02500564700225993, 75.40660817806873695 ) ) ;
#3971 = CARTESIAN_POINT ( 'NONE',  ( -4.500660556396669065, 42.81632233694663370, 96.50808879953099506 ) ) ;
#3972 = CARTESIAN_POINT ( 'NONE',  ( -5.058133621542618030, 44.89684013992257405, 91.42996379953099506 ) ) ;
#3973 = ORIENTED_EDGE ( 'NONE', *, *, #16355, .F. ) ;
#3974 = EDGE_CURVE ( 'NONE', #8922, #9137, #9598, .T. ) ;
#3975 = CARTESIAN_POINT ( 'NONE',  ( 3.460444912181559474, 49.25145096859824889, 93.14871380123798872 ) ) ;
#3976 = FACE_OUTER_BOUND ( 'NONE', #6855, .T. ) ;
#3977 = CARTESIAN_POINT ( 'NONE',  ( -0.1994209430448784792, 35.36759766960258844, 76.86610350541323555 ) ) ;
#3978 = PLANE ( 'NONE',  #20676 ) ;
#3979 = CARTESIAN_POINT ( 'NONE',  ( -3.943187491250720544, 40.73580453397070755, 91.58621379953098085 ) ) ;
#3980 = ORIENTED_EDGE ( 'NONE', *, *, #2413, .T. ) ;
#3981 = DIRECTION ( 'NONE',  ( 3.893792155548169402E-16, 7.183611964723547524E-17, -1.000000000000000000 ) ) ;
#3982 = CARTESIAN_POINT ( 'NONE',  ( 3.460444912181559474, 49.25145096859824889, 95.64871380123798872 ) ) ;
#3983 = EDGE_CURVE ( 'NONE', #6157, #12496, #14258, .T. ) ;
#3984 = ORIENTED_EDGE ( 'NONE', *, *, #11293, .F. ) ;
#3985 = CARTESIAN_POINT ( 'NONE',  ( 2.522153740306509295, 49.81903562097208038, 61.15433879953099705 ) ) ;
#3986 = DIRECTION ( 'NONE',  ( 1.000000000000000000, 1.402518428993831676E-16, 0.000000000000000000 ) ) ;
#3987 = CARTESIAN_POINT ( 'NONE',  ( 6.198496396448986090, 45.68315280215533392, 91.58621380123798872 ) ) ;
#3988 = SHAPE_DEFINITION_REPRESENTATION ( #19556, #9056 ) ;
#3989 = CARTESIAN_POINT ( 'NONE',  ( -4.895069120933020379, 37.22325107503680641, 76.32271929704664615 ) ) ;
#3990 = EDGE_CURVE ( 'NONE', #16241, #20542, #15669, .T. ) ;
#3991 = CARTESIAN_POINT ( 'NONE',  ( 0.3329060540236485899, 52.96014621323875815, 78.59782805397716743 ) ) ;
#3992 = VECTOR ( 'NONE', #17217, 1000.000000000000000 ) ;
#3993 = CARTESIAN_POINT ( 'NONE',  ( 2.522153740306509739, 50.16218137147969713, 61.15433879953099705 ) ) ;
#3994 = ORIENTED_EDGE ( 'NONE', *, *, #6614, .F. ) ;
#3995 = ORIENTED_EDGE ( 'NONE', *, *, #20174, .F. ) ;
#3996 = CARTESIAN_POINT ( 'NONE',  ( 0.7219634870551158157, 52.21250224913298155, 75.36169494263242541 ) ) ;
#3997 = VECTOR ( 'NONE', #553, 1000.000000000000000 ) ;
#3998 = EDGE_LOOP ( 'NONE', ( #8038, #11363, #17206, #18751 ) ) ;
#3999 = DIRECTION ( 'NONE',  ( -1.000000000000000000, 1.110223024625156540E-16, 6.575695984913707633E-33 ) ) ;
#4000 = DIRECTION ( 'NONE',  ( -0.7071067811865435759, 0.7071067811865515695, 0.000000000000000000 ) ) ;
#4001 = CARTESIAN_POINT ( 'NONE',  ( -4.524181921268124462, 40.28999182795290324, 96.19558880123798872 ) ) ;
#4002 = ORIENTED_EDGE ( 'NONE', *, *, #17038, .T. ) ;
#4003 = ORIENTED_EDGE ( 'NONE', *, *, #9244, .T. ) ;
#4004 = CARTESIAN_POINT ( 'NONE',  ( 6.554687423727395768, 50.64660634980899090, 79.34836068132329956 ) ) ;
#4005 = VERTEX_POINT ( 'NONE', #16081 ) ;
#4006 = CARTESIAN_POINT ( 'NONE',  ( 6.531299583006453524, 48.82481648921748274, 75.45433879953087342 ) ) ;
#4007 = DIRECTION ( 'NONE',  ( 0.2848220354341971516, -0.9585804129707224952, -1.280380753214897429E-16 ) ) ;
#4008 = VECTOR ( 'NONE', #17372, 1000.000000000000000 ) ;
#4009 = CARTESIAN_POINT ( 'NONE',  ( 2.263363662449282110, 49.77488197367689793, 93.03606768333816035 ) ) ;
#4010 = CARTESIAN_POINT ( 'NONE',  ( -2.544431595712045358, 37.47609611642828753, 76.62933879953087057 ) ) ;
#4011 = PLANE ( 'NONE',  #19781 ) ;
#4012 = CARTESIAN_POINT ( 'NONE',  ( -3.754515857360592346, 38.36993661534067712, 78.93669174070734584 ) ) ;
#4013 = CARTESIAN_POINT ( 'NONE',  ( 0.7871607343966636749, 52.96398990456528111, 77.46299673659909502 ) ) ;
#4014 = CARTESIAN_POINT ( 'NONE',  ( 2.196363144981350768, 38.51593444236233665, 92.55433879953095300 ) ) ;
#4015 = CARTESIAN_POINT ( 'NONE',  ( -3.943187491250720544, 40.73580453397070755, 94.39871380294499659 ) ) ;
#4016 = CARTESIAN_POINT ( 'NONE',  ( -2.904223097202481174, 48.62752260303690122, 91.58621380294496817 ) ) ;
#4017 = PLANE ( 'NONE',  #20795 ) ;
#4018 = CARTESIAN_POINT ( 'NONE',  ( 8.373815933025275271, 41.81065766626294788, 78.71610475470291135 ) ) ;
#4019 = VECTOR ( 'NONE', #2376, 1000.000000000000000 ) ;
#4020 = ORIENTED_EDGE ( 'NONE', *, *, #14005, .T. ) ;
#4021 = CARTESIAN_POINT ( 'NONE',  ( 8.385679600361122255, 39.92613824206362949, 77.13595644658970230 ) ) ;
#4022 = CARTESIAN_POINT ( 'NONE',  ( 0.5221537403065078520, 50.16218137147969713, 69.15433879953098995 ) ) ;
#4023 = CARTESIAN_POINT ( 'NONE',  ( -3.373742936343101739, 52.19408846175863204, 78.58955347608575437 ) ) ;
#4024 = CARTESIAN_POINT ( 'NONE',  ( 1.352400422481993658, 50.46853102219002096, 93.22683880123798872 ) ) ;
#4025 = EDGE_CURVE ( 'NONE', #18137, #14483, #1088, .T. ) ;
#4026 = CARTESIAN_POINT ( 'NONE',  ( 23.03948732994508575, 45.16218137147969003, 78.30433879953099563 ) ) ;
#4027 = CARTESIAN_POINT ( 'NONE',  ( -7.587684248800459663, 47.67520643615086584, 78.88364539996459257 ) ) ;
#4028 = DIRECTION ( 'NONE',  ( 1.540237394707284220E-16, 1.793354297423764243E-16, -1.000000000000000000 ) ) ;
#4029 = ADVANCED_FACE ( 'NONE', ( #20941 ), #11091, .T. ) ;
#4030 = CARTESIAN_POINT ( 'NONE',  ( 5.748274343403736886, 51.24227120794373747, 77.94845644658968808 ) ) ;
#4031 = ORIENTED_EDGE ( 'NONE', *, *, #16018, .T. ) ;
#4032 = ORIENTED_EDGE ( 'NONE', *, *, #2356, .F. ) ;
#4033 = CARTESIAN_POINT ( 'NONE',  ( 9.279665234200917823, 42.60546990007262025, 79.15097751326614173 ) ) ;
#4034 = CARTESIAN_POINT ( 'NONE',  ( -4.233737104609305746, 36.73475175465707565, 75.41196988111011024 ) ) ;
#4035 = EDGE_CURVE ( 'NONE', #8763, #1377, #7676, .T. ) ;
#4036 = DIRECTION ( 'NONE',  ( -0.000000000000000000, -1.000000000000000000, -0.000000000000000000 ) ) ;
#4037 = CARTESIAN_POINT ( 'NONE',  ( -1.219056181852248066, 49.77488197367201650, 94.56237966814981633 ) ) ;
#4038 = CARTESIAN_POINT ( 'NONE',  ( 27.03948732994508930, 43.16218137147969003, 77.50433879953099847 ) ) ;
#4039 = CIRCLE ( 'NONE', #14908, 6.999999999999999112 ) ;
#4040 = CARTESIAN_POINT ( 'NONE',  ( -0.9199438314403624029, 52.23437776363726215, 72.45433879953087342 ) ) ;
#4041 = CARTESIAN_POINT ( 'NONE',  ( 0.5221537403065181771, 44.16218137147969003, 56.15433879953099705 ) ) ;
#4042 = CARTESIAN_POINT ( 'NONE',  ( -1.219503646467429814, 49.90383875825364157, 53.41268141275706682 ) ) ;
#4043 = CARTESIAN_POINT ( 'NONE',  ( -1.219503646467433144, 49.90383875825363447, 85.41268141275706682 ) ) ;
#4044 = DIRECTION ( 'NONE',  ( -1.334402673828313339E-16, -1.619179559944692391E-32, 1.000000000000000000 ) ) ;
#4045 = CARTESIAN_POINT ( 'NONE',  ( 6.882736312352589536, 37.89144858414100270, 76.69330938776616335 ) ) ;
#4046 = ORIENTED_EDGE ( 'NONE', *, *, #2595, .T. ) ;
#4047 = DIRECTION ( 'NONE',  ( 1.000000000000000000, 0.000000000000000000, 0.000000000000000000 ) ) ;
#4048 = AXIS2_PLACEMENT_3D ( 'NONE', #1994, #10417, #18063 ) ;
#4049 = VERTEX_POINT ( 'NONE', #4668 ) ;
#4050 = CARTESIAN_POINT ( 'NONE',  ( -4.449342498592997686, 50.67858896256802836, 78.59458524649963351 ) ) ;
#4051 = B_SPLINE_CURVE_WITH_KNOTS ( 'NONE', 3,
 ( #10673, #18731, #6054, #13942, #12452, #15542, #748, #10769, #1070, #2558, #18932, #12250, #3931, #15335, #2457 ),
 .UNSPECIFIED., .F., .F.,
 ( 4, 1, 1, 1, 1, 1, 1, 1, 1, 1, 1, 1, 4 ),
 ( 0.000000000000000000, 0.07577303389073718198, 0.1558117613168219784, 0.2417361372947465226, 0.3357870204060591224, 0.3882587240527491379, 0.4455552461494497463, 0.5113167710153618817, 0.5866953322903324386, 0.6731791507778834838, 0.7705825181721650541, 0.8794626622360116608, 1.000000000000000000 ),
 .UNSPECIFIED. ) ;
#4052 = CARTESIAN_POINT ( 'NONE',  ( -4.500660556396669065, 42.81632233694663370, 95.57058880294496817 ) ) ;
#4053 = EDGE_LOOP ( 'NONE', ( #286, #3613, #1559, #16718, #8157, #19812, #1720, #7299 ) ) ;
#4054 = CARTESIAN_POINT ( 'NONE',  ( 5.052198367669454626, 48.31320248322255395, 93.42308879782402187 ) ) ;
#4056 = CIRCLE ( 'NONE', #17653, 8.199999999999995737 ) ;
#4055 = CARTESIAN_POINT ( 'NONE',  ( -0.1709386726045610538, 50.28109722957944427, 59.67325465763076409 ) ) ;
#4057 = AXIS2_PLACEMENT_3D ( 'NONE', #9842, #15045, #5027 ) ;
#4058 = CARTESIAN_POINT ( 'NONE',  ( -4.370691255933373931, 51.48170569318705247, 79.53937015691786883 ) ) ;
#4059 = DIRECTION ( 'NONE',  ( -1.000000000000000000, 1.134288711164059691E-16, -3.893792155548169402E-16 ) ) ;
#4060 = CARTESIAN_POINT ( 'NONE',  ( 5.308257127890501970, 50.81265825806588055, 77.27261723006257910 ) ) ;
#4061 = EDGE_CURVE ( 'NONE', #16593, #18224, #20739, .T. ) ;
#4062 = DIRECTION ( 'NONE',  ( 0.000000000000000000, 0.000000000000000000, 1.000000000000000000 ) ) ;
#4063 = ORIENTED_EDGE ( 'NONE', *, *, #2624, .F. ) ;
#4064 = CARTESIAN_POINT ( 'NONE',  ( 8.234060390202110113, 41.37527878033370854, 77.44800974218487966 ) ) ;
#4065 = VERTEX_POINT ( 'NONE', #18949 ) ;
#4066 = LINE ( 'NONE', #2686, #20328 ) ;
#4067 = CARTESIAN_POINT ( 'NONE',  ( 1.658154530501163126, 36.04125148601230677, 79.45433879953087342 ) ) ;
#4068 = CARTESIAN_POINT ( 'NONE',  ( -7.171016202898661263, 41.77105925685706467, 76.16022115247204738 ) ) ;
#4069 = VECTOR ( 'NONE', #4638, 1000.000000000000000 ) ;
#4070 = PLANE ( 'NONE',  #10591 ) ;
#4071 = CARTESIAN_POINT ( 'NONE',  ( 6.761793986577667503, 50.49362507459272820, 79.13556070921569585 ) ) ;
#4072 = LINE ( 'NONE', #1206, #7069 ) ;
#4073 = CARTESIAN_POINT ( 'NONE',  ( 2.463659247115866258, 38.82793883177424732, 94.28246379782397923 ) ) ;
#4074 = LINE ( 'NONE', #788, #2454 ) ;
#4075 = B_SPLINE_SURFACE_WITH_KNOTS ( 'NONE', 3, 1, ( 
 ( #5511, #13398 ),
 ( #2433, #11912 ),
 ( #16799, #407 ),
 ( #5614, #5188 ),
 ( #18387, #7093 ),
 ( #8929, #12118 ),
 ( #15418, #13709 ),
 ( #15099, #6894 ),
 ( #15311, #4013 ),
 ( #12023, #2320 ),
 ( #3696, #3807 ),
 ( #613, #11705 ),
 ( #18599, #13596 ),
 ( #2217, #3598 ),
 ( #16588, #8816 ) ),
 .UNSPECIFIED., .F., .F., .F.,
 ( 4, 1, 1, 1, 1, 1, 1, 1, 1, 1, 1, 1, 4 ),
 ( 2, 2 ),
 ( 0.000000000000000000, 0.1162067238869137348, 0.2214153483095009645, 0.3146488149876708329, 0.3978441427673392039, 0.4713237328820706895, 0.5351740646982715566, 0.5914750994871406098, 0.6429785647885755129, 0.7385262294747835243, 0.8287699788399466305, 0.9143335036940697380, 1.000000000000000000 ),
 ( 0.000000000000000000, 1.000000000000000000 ),
 .UNSPECIFIED. ) ;
#4076 = AXIS2_PLACEMENT_3D ( 'NONE', #239, #8123, #13026 ) ;
#4077 = ORIENTED_EDGE ( 'NONE', *, *, #9773, .T. ) ;
#4078 = CARTESIAN_POINT ( 'NONE',  ( 4.271559758984892596, 51.45486941304334749, 77.47147465385867804 ) ) ;
#4079 = VERTEX_POINT ( 'NONE', #20637 ) ;
#4080 = CARTESIAN_POINT ( 'NONE',  ( 29.63948732994508006, 36.35905713404685002, 74.70433879953100131 ) ) ;
#4081 = CARTESIAN_POINT ( 'NONE',  ( -3.943187491250720544, 40.73580453397070755, 95.33621379953099506 ) ) ;
#4082 =( GEOMETRIC_REPRESENTATION_CONTEXT ( 3 ) GLOBAL_UNCERTAINTY_ASSIGNED_CONTEXT ( ( #4853 ) ) GLOBAL_UNIT_ASSIGNED_CONTEXT ( ( #4544, #14441, #20817 ) ) REPRESENTATION_CONTEXT ( 'NONE', 'WORKASPACE' ) );
#4083 = ORIENTED_EDGE ( 'NONE', *, *, #16747, .T. ) ;
#4084 = CARTESIAN_POINT ( 'NONE',  ( -0.9988176903691428077, 49.83852402762217082, 93.30496380123798872 ) ) ;
#4085 = CARTESIAN_POINT ( 'NONE',  ( 2.122153740306511605, 49.76218137147969856, 61.55433879953100273 ) ) ;
#4086 = CARTESIAN_POINT ( 'NONE',  ( 3.403907234131700488, 40.01403842974062997, 95.05433879953098142 ) ) ;
#4087 = CARTESIAN_POINT ( 'NONE',  ( -7.677846259693483333, 47.36218137147966445, 93.55433879953098142 ) ) ;
#4088 = ORIENTED_EDGE ( 'NONE', *, *, #19493, .T. ) ;
#4089 = CARTESIAN_POINT ( 'NONE',  ( 0.7398053571154690200, 52.35989412137791277, 79.54697819541583215 ) ) ;
#4090 = CARTESIAN_POINT ( 'NONE',  ( 3.460444912181559474, 49.25145096859824889, 93.14871380123798872 ) ) ;
#4091 = VECTOR ( 'NONE', #12366, 1000.000000000000000 ) ;
#4092 = VERTEX_POINT ( 'NONE', #19254 ) ;
#4093 = CARTESIAN_POINT ( 'NONE',  ( -1.549594827053651924, 39.36475212009352020, 92.45433879953094447 ) ) ;
#4094 = CARTESIAN_POINT ( 'NONE',  ( -1.477846259693502917, 47.62628298661744708, 77.15433879953100416 ) ) ;
#4095 = FACE_OUTER_BOUND ( 'NONE', #19308, .T. ) ;
#4096 = APPLICATION_PROTOCOL_DEFINITION ( 'draft international standard', 'automotive_design', 1998, #2614 ) ;
#4097 = LINE ( 'NONE', #13784, #10692 ) ;
#4098 = CARTESIAN_POINT ( 'NONE',  ( 5.599231707071657738, 51.35236299959863970, 78.59183879953087626 ) ) ;
#4099 = EDGE_CURVE ( 'NONE', #8069, #1372, #12467, .T. ) ;
#4100 = CARTESIAN_POINT ( 'NONE',  ( -4.477846259693498254, 51.36218137147968577, 53.35433879953099989 ) ) ;
#4101 = ORIENTED_EDGE ( 'NONE', *, *, #5348, .F. ) ;
#4102 = CARTESIAN_POINT ( 'NONE',  ( 2.084502445282489624, 52.95459623993866671, 76.15080458372598571 ) ) ;
#4103 = ORIENTED_EDGE ( 'NONE', *, *, #16099, .T. ) ;
#4104 = CARTESIAN_POINT ( 'NONE',  ( 6.961592395446249526, 50.34604203833234237, 76.59575135851817151 ) ) ;
#4105 = CARTESIAN_POINT ( 'NONE',  ( -5.677846259693490438, 44.16218137147969003, 92.55433879953098142 ) ) ;
#4106 = CARTESIAN_POINT ( 'NONE',  ( 5.146043734657006041, 40.41782908280415398, 90.30634084312077903 ) ) ;
#4107 = EDGE_LOOP ( 'NONE', ( #4101, #9897, #9705, #15167 ) ) ;
#4108 = DIRECTION ( 'NONE',  ( 0.000000000000000000, 3.469446951953617147E-16, 1.000000000000000000 ) ) ;
#4109 = VECTOR ( 'NONE', #7880, 1000.000000000000000 ) ;
#4110 = ORIENTED_EDGE ( 'NONE', *, *, #4617, .F. ) ;
#4111 = CARTESIAN_POINT ( 'NONE',  ( 2.538045550429134600, 49.87014351810298507, 75.45433879953087342 ) ) ;
#4112 = DIRECTION ( 'NONE',  ( -1.779391786395883536E-16, -5.922860397471806844E-17, 1.000000000000000000 ) ) ;
#4113 = CARTESIAN_POINT ( 'NONE',  ( 7.795054281054241585, 40.53718145105147386, 75.64968528315669971 ) ) ;
#4114 = CYLINDRICAL_SURFACE ( 'NONE', #4966, 0.6000000000000033085 ) ;
#4115 = FACE_OUTER_BOUND ( 'NONE', #14509, .T. ) ;
#4116 = CARTESIAN_POINT ( 'NONE',  ( -7.313565574299385474, 41.74526126053015673, 79.54845644658969661 ) ) ;
#4117 = DIRECTION ( 'NONE',  ( 0.8191520442889931308, 0.5735764363510443831, 1.093078678171161523E-16 ) ) ;
#4118 = CYLINDRICAL_SURFACE ( 'NONE', #11815, 4.200000000000000178 ) ;
#4119 = CARTESIAN_POINT ( 'NONE',  ( -5.784195910403845176, 44.99242805365518194, 92.13308880123798872 ) ) ;
#4120 = CARTESIAN_POINT ( 'NONE',  ( -5.364198675898909308, 49.85200608322956128, 76.15119298917683466 ) ) ;
#4121 = CARTESIAN_POINT ( 'NONE',  ( 4.987469076889843755, 50.87941446422544090, 75.37972891991934432 ) ) ;
#4122 = CARTESIAN_POINT ( 'NONE',  ( -0.2125050281363792815, 38.58189400963055959, 93.30496380294501080 ) ) ;
#4123 = EDGE_CURVE ( 'NONE', #468, #7741, #4471, .T. ) ;
#4124 = VECTOR ( 'NONE', #15508, 999.9999999999998863 ) ;
#4125 = DIRECTION ( 'NONE',  ( 1.540237394707284220E-16, 1.793354297423764243E-16, -1.000000000000000000 ) ) ;
#4126 = CARTESIAN_POINT ( 'NONE',  ( 8.882918921757626762, 41.41639603256331981, 78.93548851266230315 ) ) ;
#4127 = VECTOR ( 'NONE', #4811, 1000.000000000000000 ) ;
#4128 =( BOUNDED_CURVE ( )  B_SPLINE_CURVE ( 3, ( #7894, #14165, #17262, #4269 ),
 .UNSPECIFIED., .F., .F. ) 
 B_SPLINE_CURVE_WITH_KNOTS ( ( 4, 4 ),
 ( 4.188790204786388749, 4.300872134317200945 ),
 .UNSPECIFIED. ) 
 CURVE ( )  GEOMETRIC_REPRESENTATION_ITEM ( )  RATIONAL_B_SPLINE_CURVE ( ( 1.000000000000000000, 0.9989534107080366709, 0.9989534107080366709, 1.000000000000000000 ) ) 
 REPRESENTATION_ITEM ( '' )  );
#4129 = ORIENTED_EDGE ( 'NONE', *, *, #12758, .F. ) ;
#4130 = FACE_BOUND ( 'NONE', #4588, .T. ) ;
#4131 = LINE ( 'NONE', #18288, #9261 ) ;
#4132 = CARTESIAN_POINT ( 'NONE',  ( -3.778837258911088792, 51.90462289030131160, 79.34012906335151172 ) ) ;
#4133 = CARTESIAN_POINT ( 'NONE',  ( 4.454345183533989783, 39.79502090995749342, 90.27410581162071423 ) ) ;
#4134 = DIRECTION ( 'NONE',  ( -0.000000000000000000, -0.000000000000000000, -1.000000000000000000 ) ) ;
#4135 = LINE ( 'NONE', #9157, #13688 ) ;
#4136 = DIRECTION ( 'NONE',  ( 1.540237394707284220E-16, 1.793354297423764243E-16, -1.000000000000000000 ) ) ;
#4137 = ADVANCED_FACE ( 'NONE', ( #9490 ), #20846, .T. ) ;
#4138 = DIRECTION ( 'NONE',  ( -0.3165065846431826535, -0.9485903129789529098, -2.188653791613874008E-16 ) ) ;
#4139 = ORIENTED_EDGE ( 'NONE', *, *, #2723, .T. ) ;
#4140 = EDGE_CURVE ( 'NONE', #13663, #18483, #14973, .T. ) ;
#4141 = VECTOR ( 'NONE', #17010, 1000.000000000000000 ) ;
#4142 = CARTESIAN_POINT ( 'NONE',  ( 8.617743499586005385, 42.98606652041282672, 78.90414333341678343 ) ) ;
#4143 = CARTESIAN_POINT ( 'NONE',  ( 2.522153740306506187, 49.81903562097208038, 77.15433879953100416 ) ) ;
#4144 = LINE ( 'NONE', #5953, #1109 ) ;
#4145 = AXIS2_PLACEMENT_3D ( 'NONE', #6595, #6701, #16717 ) ;
#4146 = CARTESIAN_POINT ( 'NONE',  ( -4.567115856812060670, 47.10047254335474065, 94.71121380123797451 ) ) ;
#4147 = CARTESIAN_POINT ( 'NONE',  ( -4.898948001865909063, 44.60983979649643771, 95.05433879953105247 ) ) ;
#4148 = DIRECTION ( 'NONE',  ( -1.540237394707284220E-16, -1.793354297423764243E-16, 1.000000000000000000 ) ) ;
#4149 = CARTESIAN_POINT ( 'NONE',  ( 4.987494971863720927, 47.58855820898865829, 93.77371380294498238 ) ) ;
#4150 = CARTESIAN_POINT ( 'NONE',  ( -0.9988176903691428077, 49.83852402762217082, 93.14871380123798872 ) ) ;
#4151 = EDGE_CURVE ( 'NONE', #12841, #18903, #6174, .T. ) ;
#4152 = EDGE_CURVE ( 'NONE', #10420, #14607, #7990, .T. ) ;
#4153 = EDGE_CURVE ( 'NONE', #10457, #14370, #20728, .T. ) ;
#4154 = DIRECTION ( 'NONE',  ( 1.000000000000000000, -0.000000000000000000, -0.000000000000000000 ) ) ;
#4155 = LINE ( 'NONE', #18840, #10193 ) ;
#4156 = CARTESIAN_POINT ( 'NONE',  ( -5.403476264047557542, 38.53479744785971661, 79.12851299606570876 ) ) ;
#4157 = VECTOR ( 'NONE', #16710, 1000.000000000000000 ) ;
#4158 = CARTESIAN_POINT ( 'NONE',  ( 6.268485860042931179, 37.45252770006494103, 75.44618574453703275 ) ) ;
#4159 = ORIENTED_EDGE ( 'NONE', *, *, #3250, .F. ) ;
#4160 = EDGE_CURVE ( 'NONE', #14337, #18484, #19158, .T. ) ;
#4161 = AXIS2_PLACEMENT_3D ( 'NONE', #611, #20397, #10430 ) ;
#4162 = CARTESIAN_POINT ( 'NONE',  ( 4.048141534226263438, 36.75897868094575216, 79.45433879953087342 ) ) ;
#4163 = ORIENTED_EDGE ( 'NONE', *, *, #8621, .T. ) ;
#4164 = CARTESIAN_POINT ( 'NONE',  ( 0.5221537403064979710, 39.16218137147969003, 93.35386871425482980 ) ) ;
#4165 = CARTESIAN_POINT ( 'NONE',  ( -4.567115856812060670, 47.10047254335474065, 90.80496380123797451 ) ) ;
#4166 = ORIENTED_EDGE ( 'NONE', *, *, #10308, .T. ) ;
#4167 = LINE ( 'NONE', #12470, #12689 ) ;
#4168 = CARTESIAN_POINT ( 'NONE',  ( -0.2125050281363792815, 38.58189400963056670, 94.24246379953099506 ) ) ;
#4169 = CARTESIAN_POINT ( 'NONE',  ( -3.042256558752230777, 51.51118090841579544, 79.00686454089694166 ) ) ;
#4170 = CARTESIAN_POINT ( 'NONE',  ( -0.1709386726045608318, 50.28109722957944427, 75.67325465763074988 ) ) ;
#4171 = CARTESIAN_POINT ( 'NONE',  ( 5.201902455060544384, 50.89121817065782238, 77.00567114208729436 ) ) ;
#4172 = CARTESIAN_POINT ( 'NONE',  ( -4.200570128010908455, 37.62426765031928966, 79.54612747205591461 ) ) ;
#4173 = ORIENTED_EDGE ( 'NONE', *, *, #20241, .F. ) ;
#4174 = LINE ( 'NONE', #9082, #19698 ) ;
#4175 = AXIS2_PLACEMENT_3D ( 'NONE', #8409, #8728, #19780 ) ;
#4176 = ORIENTED_EDGE ( 'NONE', *, *, #19769, .F. ) ;
#4177 = DIRECTION ( 'NONE',  ( 0.000000000000000000, -1.000000000000000000, 0.000000000000000000 ) ) ;
#4178 = LINE ( 'NONE', #1494, #14158 ) ;
#4179 = DIRECTION ( 'NONE',  ( 0.007885122365275663500, 0.9999689119394085113, 1.805443505845543142E-16 ) ) ;
#4180 = CARTESIAN_POINT ( 'NONE',  ( 6.907457231639352102, 50.38602950313908480, 78.73390793106847241 ) ) ;
#4181 = FACE_OUTER_BOUND ( 'NONE', #1981, .T. ) ;
#4182 = CARTESIAN_POINT ( 'NONE',  ( -4.722163902562435567, 37.85776514764631173, 77.90206145538023463 ) ) ;
#4183 = EDGE_CURVE ( 'NONE', #6991, #7247, #3096, .T. ) ;
#4184 = CARTESIAN_POINT ( 'NONE',  ( 5.037341483232629535, 37.31725042616477594, 78.09625056423675460 ) ) ;
#4185 = ORIENTED_EDGE ( 'NONE', *, *, #8470, .T. ) ;
#4186 = EDGE_CURVE ( 'NONE', #8801, #4661, #4776, .T. ) ;
#4187 = CARTESIAN_POINT ( 'NONE',  ( 8.211813679349305062, 41.32530918129923947, 78.64407474691132904 ) ) ;
#4188 = ORIENTED_EDGE ( 'NONE', *, *, #494, .T. ) ;
#4189 = VECTOR ( 'NONE', #10674, 1000.000000000000000 ) ;
#4190 = FACE_OUTER_BOUND ( 'NONE', #6183, .T. ) ;
#4191 = CARTESIAN_POINT ( 'NONE',  ( -3.943187491250720544, 40.73580453397070755, 91.58621379953098085 ) ) ;
#4192 = VERTEX_POINT ( 'NONE', #8092 ) ;
#4193 = CARTESIAN_POINT ( 'NONE',  ( 3.460444912181559474, 49.25145096859824889, 91.89871380123798872 ) ) ;
#4194 = CARTESIAN_POINT ( 'NONE',  ( -4.305671849203691615, 50.60821918116168661, 79.54427050475041483 ) ) ;
#4195 = CARTESIAN_POINT ( 'NONE',  ( 0.5221537403065364957, 44.16218137147969003, 123.5543387995310098 ) ) ;
#4196 = CARTESIAN_POINT ( 'NONE',  ( -1.987575841473666394, 39.35622280378359505, 95.05433879953096721 ) ) ;
#4197 = LINE ( 'NONE', #12189, #8831 ) ;
#4198 = EDGE_CURVE ( 'NONE', #19989, #618, #12966, .T. ) ;
#4199 = ORIENTED_EDGE ( 'NONE', *, *, #4525, .F. ) ;
#4200 = DIRECTION ( 'NONE',  ( -1.540237394707284220E-16, -1.793354297423764243E-16, 1.000000000000000000 ) ) ;
#4201 = CARTESIAN_POINT ( 'NONE',  ( 0.6026978026911212760, 52.96544839334315924, 78.93607282253582014 ) ) ;
#4202 = ORIENTED_EDGE ( 'NONE', *, *, #20540, .T. ) ;
#4203 = CARTESIAN_POINT ( 'NONE',  ( -4.787608953476067519, 50.41169371076171046, 79.45199527959816521 ) ) ;
#4204 = CARTESIAN_POINT ( 'NONE',  ( 1.119863296874942460, 50.25084051303456789, 85.06567965797613340 ) ) ;
#4205 = CIRCLE ( 'NONE', #16103, 0.5999999999999928724 ) ;
#4206 = PRODUCT_CONTEXT ( 'NONE', #435, 'mechanical' ) ;
#4207 = CARTESIAN_POINT ( 'NONE',  ( 5.265323063642338930, 37.48261972611145865, 75.97391373086902888 ) ) ;
#4208 = CARTESIAN_POINT ( 'NONE',  ( 5.438900134727234992, 36.85973611382630821, 76.29939265556315320 ) ) ;
#4209 = DIRECTION ( 'NONE',  ( -1.540237394707284467E-16, -1.793354297423764243E-16, 1.000000000000000000 ) ) ;
#4210 = ORIENTED_EDGE ( 'NONE', *, *, #7498, .T. ) ;
#4211 = CARTESIAN_POINT ( 'NONE',  ( -6.899669779797631186, 47.65063352677621822, 78.32453850483534552 ) ) ;
#4212 = ORIENTED_EDGE ( 'NONE', *, *, #5834, .F. ) ;
#4213 = CARTESIAN_POINT ( 'NONE',  ( 6.241727703577843123, 50.87777708829695200, 75.41423045364997790 ) ) ;
#4214 = DIRECTION ( 'NONE',  ( 1.000000000000000000, 0.000000000000000000, -0.000000000000000000 ) ) ;
#4215 = CARTESIAN_POINT ( 'NONE',  ( -4.524181921268124462, 40.28999182795290324, 96.03933880123798872 ) ) ;
#4216 = ORIENTED_EDGE ( 'NONE', *, *, #6101, .F. ) ;
#4217 = CARTESIAN_POINT ( 'NONE',  ( 0.5221537403065056315, 44.16218137147969713, 77.55433879953099563 ) ) ;
#4218 = EDGE_LOOP ( 'NONE', ( #2917, #1856, #9625, #15410, #12660 ) ) ;
#4219 = CARTESIAN_POINT ( 'NONE',  ( 4.719835101441633540, 52.00193784792148222, 79.11209812681292419 ) ) ;
#4220 = CARTESIAN_POINT ( 'NONE',  ( 2.522153740306492864, 49.81903562097208749, 51.21119304902340019 ) ) ;
#4221 = CARTESIAN_POINT ( 'NONE',  ( 8.435567168294131335, 40.07565444796716747, 75.89798363837520867 ) ) ;
#4222 = CARTESIAN_POINT ( 'NONE',  ( -1.392380047608630544, 49.84925249003584469, 61.23980501161588563 ) ) ;
#4223 = CARTESIAN_POINT ( 'NONE',  ( -6.705289424168793921, 40.29829583493234679, 78.54487611535471103 ) ) ;
#4224 = CARTESIAN_POINT ( 'NONE',  ( -7.413538919509569780, 42.09506629875884443, 79.52729148488525368 ) ) ;
#4225 = LINE ( 'NONE', #13806, #16776 ) ;
#4226 = CARTESIAN_POINT ( 'NONE',  ( 5.902048492000326441, 51.12868443877599134, 78.27786821129558348 ) ) ;
#4227 = CARTESIAN_POINT ( 'NONE',  ( -6.850209527372854268, 47.75220363455441230, 78.32492703482499508 ) ) ;
#4228 = CARTESIAN_POINT ( 'NONE',  ( 5.333527369480803415, 51.54862809055342154, 75.39573407869305299 ) ) ;
#4229 = CARTESIAN_POINT ( 'NONE',  ( -5.058133621542618030, 44.89684013992257405, 92.99246380294498238 ) ) ;
#4230 = CARTESIAN_POINT ( 'NONE',  ( -2.083470957239373256, 47.45622447009557021, 82.45433879953087342 ) ) ;
#4231 = VERTEX_POINT ( 'NONE', #6 ) ;
#4232 = DIRECTION ( 'NONE',  ( 0.5813877811927012917, -0.8136266022444372803, -5.636455622144620416E-17 ) ) ;
#4233 = CARTESIAN_POINT ( 'NONE',  ( -3.154801521863568325, 47.83913663364971569, 92.55433879953098142 ) ) ;
#4234 = CARTESIAN_POINT ( 'NONE',  ( -4.410496611078632334, 50.71268463827564688, 78.87432127096172962 ) ) ;
#4235 = CARTESIAN_POINT ( 'NONE',  ( 5.146040402138061687, 40.41782331071202350, 90.30634062920465510 ) ) ;
#4236 = CARTESIAN_POINT ( 'NONE',  ( -2.416137431568557314, 39.07291177436112406, 93.77371380123797451 ) ) ;
#4237 = CARTESIAN_POINT ( 'NONE',  ( -7.945817805444411519, 41.74005988965458869, 79.54527856538405217 ) ) ;
#4238 = CARTESIAN_POINT ( 'NONE',  ( 5.428124502387796646, 36.85203624147762724, 77.45531005930804724 ) ) ;
#4239 = EDGE_CURVE ( 'NONE', #10226, #13351, #13410, .T. ) ;
#4240 = DIRECTION ( 'NONE',  ( -5.626130192357176673E-16, -1.831515347669941892E-30, 1.000000000000000000 ) ) ;
#4241 = PLANE ( 'NONE',  #2628 ) ;
#4242 = LINE ( 'NONE', #20203, #6860 ) ;
#4243 = CARTESIAN_POINT ( 'NONE',  ( 5.839579929017896021, 51.17482744986389775, 77.27318761637275202 ) ) ;
#4244 = B_SPLINE_SURFACE_WITH_KNOTS ( 'NONE', 3, 1, ( 
 ( #10225, #417 ),
 ( #16807, #15108 ),
 ( #16702, #18503 ),
 ( #15207, #11612 ),
 ( #5095, #16594 ),
 ( #2126, #11920 ),
 ( #619, #7099 ),
 ( #13605, #13498 ),
 ( #514, #2015 ),
 ( #19873, #19971 ),
 ( #20081, #8514 ),
 ( #10441, #10014 ),
 ( #5294, #5398 ),
 ( #5519, #1819 ),
 ( #8301, #16491 ) ),
 .UNSPECIFIED., .F., .F., .F.,
 ( 4, 1, 1, 1, 1, 1, 1, 1, 1, 1, 1, 1, 4 ),
 ( 2, 2 ),
 ( 0.000000000000000000, 0.07541797170168144937, 0.1450771083642982684, 0.2121257487690652588, 0.2760806684033449421, 0.3377115757710241750, 0.3948710521788694749, 0.4527877999541435883, 0.5116051076384522389, 0.5882781613054922643, 0.6941869364785798746, 0.8318120212073902842, 1.000000000000000000 ),
 ( 0.000000000000000000, 1.000000000000000000 ),
 .UNSPECIFIED. ) ;
#4245 = LINE ( 'NONE', #7872, #592 ) ;
#4246 = CARTESIAN_POINT ( 'NONE',  ( -4.032264951078913029, 50.98107207184723677, 78.45066232894264147 ) ) ;
#4247 = DIRECTION ( 'NONE',  ( 0.3330135628418984250, 0.9429220365244121993, 2.203913228770417655E-16 ) ) ;
#4248 = CARTESIAN_POINT ( 'NONE',  ( 5.568489401881125289, 48.03437091500646261, 92.91433880123798872 ) ) ;
#4249 =( BOUNDED_CURVE ( )  B_SPLINE_CURVE ( 3, ( #1699, #8178, #14665, #3079 ),
 .UNSPECIFIED., .F., .F. ) 
 B_SPLINE_CURVE_WITH_KNOTS ( ( 4, 4 ),
 ( 1.982313172862385731, 2.094395102393197483 ),
 .UNSPECIFIED. ) 
 CURVE ( )  GEOMETRIC_REPRESENTATION_ITEM ( )  RATIONAL_B_SPLINE_CURVE ( ( 1.000000000000000000, 0.9989534107080366709, 0.9989534107080366709, 1.000000000000000000 ) ) 
 REPRESENTATION_ITEM ( '' )  );
#4250 = CARTESIAN_POINT ( 'NONE',  ( -4.383767596367525776, 51.47236181906818331, 76.38961819735682468 ) ) ;
#4251 = ADVANCED_FACE ( 'NONE', ( #19672 ), #13764, .T. ) ;
#4252 = CARTESIAN_POINT ( 'NONE',  ( -7.084038296528465395, 47.03879614692494471, 78.06303731277932911 ) ) ;
#4253 = CARTESIAN_POINT ( 'NONE',  ( 11.22215374030649926, 39.96218137147969429, 80.55433879953099563 ) ) ;
#4254 = DIRECTION ( 'NONE',  ( 1.084202172485505420E-16, 1.000000000000000000, 0.000000000000000000 ) ) ;
#4255 = ORIENTED_EDGE ( 'NONE', *, *, #5063, .T. ) ;
#4256 = CARTESIAN_POINT ( 'NONE',  ( 5.579238239244114439, 50.61249542689395042, 76.92469047792664583 ) ) ;
#4257 = EDGE_CURVE ( 'NONE', #13330, #16250, #13093, .T. ) ;
#4258 = ORIENTED_EDGE ( 'NONE', *, *, #10583, .T. ) ;
#4259 = CARTESIAN_POINT ( 'NONE',  ( -4.790699304645749557, 51.18158331905331693, 78.75763390087725213 ) ) ;
#4260 = CARTESIAN_POINT ( 'NONE',  ( -4.500660556396669065, 42.81632233694663370, 91.82058880294496817 ) ) ;
#4261 = ORIENTED_EDGE ( 'NONE', *, *, #15524, .F. ) ;
#4262 = CARTESIAN_POINT ( 'NONE',  ( -1.876873622437039257, 39.01745058958429269, 92.87621379782399345 ) ) ;
#4263 = CARTESIAN_POINT ( 'NONE',  ( -3.943187491250720544, 40.73580453397070755, 94.08621379953100927 ) ) ;
#4264 = LINE ( 'NONE', #7994, #3026 ) ;
#4265 = CYLINDRICAL_SURFACE ( 'NONE', #1924, 5.199999999999999289 ) ;
#4266 = CARTESIAN_POINT ( 'NONE',  ( 0.8504581424305197590, 52.96356711606490819, 76.46781884397893236 ) ) ;
#4267 = CARTESIAN_POINT ( 'NONE',  ( -3.098319451127027335, 36.81007947667079350, 78.58910375170351870 ) ) ;
#4268 = EDGE_LOOP ( 'NONE', ( #6912, #17885, #18094, #12090 ) ) ;
#4269 = CARTESIAN_POINT ( 'NONE',  ( 2.122153740306507164, 47.82824192744436687, 85.55433879953100984 ) ) ;
#4270 = CARTESIAN_POINT ( 'NONE',  ( -4.812088799398939187, 42.22067586467031930, 92.56371379782397923 ) ) ;
#4271 = ORIENTED_EDGE ( 'NONE', *, *, #7673, .F. ) ;
#4272 = CARTESIAN_POINT ( 'NONE',  ( 30.92220646078100188, 42.76218137147968434, 62.80715055817104542 ) ) ;
#4273 = DIRECTION ( 'NONE',  ( 1.110223024625156540E-16, 1.000000000000000000, 5.922860397471808077E-17 ) ) ;
#4274 = CARTESIAN_POINT ( 'NONE',  ( 31.07218010054375412, 42.76218137147968434, 70.80574467885102763 ) ) ;
#4275 = CARTESIAN_POINT ( 'NONE',  ( -7.012702200122923557, 47.39982587559282479, 78.90834094864484882 ) ) ;
#4276 = LINE ( 'NONE', #1105, #5033 ) ;
#4277 = CARTESIAN_POINT ( 'NONE',  ( -1.677846259693481556, 47.73989013547935656, 56.15433879953099705 ) ) ;
#4278 = FACE_OUTER_BOUND ( 'NONE', #10735, .T. ) ;
#4279 = ORIENTED_EDGE ( 'NONE', *, *, #4880, .F. ) ;
#4280 = CARTESIAN_POINT ( 'NONE',  ( -4.804644443005473775, 51.17161863374556674, 76.44036821129557779 ) ) ;
#4281 = ORIENTED_EDGE ( 'NONE', *, *, #3886, .F. ) ;
#4282 = AXIS2_PLACEMENT_3D ( 'NONE', #16999, #7202, #10427 ) ;
#4283 = LINE ( 'NONE', #7276, #18686 ) ;
#4284 = CARTESIAN_POINT ( 'NONE',  ( 3.460444912181559474, 49.25145096859824889, 94.39871380123798872 ) ) ;
#4285 = DIRECTION ( 'NONE',  ( 1.000000000000000000, -0.000000000000000000, -0.000000000000000000 ) ) ;
#4286 = ORIENTED_EDGE ( 'NONE', *, *, #19058, .T. ) ;
#4287 = EDGE_CURVE ( 'NONE', #10061, #26, #19566, .T. ) ;
#4288 = CARTESIAN_POINT ( 'NONE',  ( 5.611423337425062385, 41.22389019960463230, 94.08621380123797451 ) ) ;
#4289 = CARTESIAN_POINT ( 'NONE',  ( -4.466244978593272741, 50.49347950185737943, 79.52300236340988704 ) ) ;
#4290 = DIRECTION ( 'NONE',  ( 0.7071067811865460184, 3.444999758574045180E-16, 0.7071067811865490160 ) ) ;
#4291 = ORIENTED_EDGE ( 'NONE', *, *, #2365, .F. ) ;
#4292 = CARTESIAN_POINT ( 'NONE',  ( 6.853565520360258567, 37.87060420419414442, 77.68698088877128782 ) ) ;
#4293 = CARTESIAN_POINT ( 'NONE',  ( 13.13948732994505875, 43.16218137147969003, 78.60433879953099279 ) ) ;
#4294 = EDGE_CURVE ( 'NONE', #11222, #7247, #9914, .T. ) ;
#4295 = EDGE_LOOP ( 'NONE', ( #8513, #2476, #6850, #7737 ) ) ;
#4296 = CARTESIAN_POINT ( 'NONE',  ( 4.393996117251955269, 36.11308595931626542, 76.73963291717792856 ) ) ;
#4297 = CARTESIAN_POINT ( 'NONE',  ( -4.524181921268124462, 40.28999182795290324, 91.19558880123797451 ) ) ;
#4298 = VERTEX_POINT ( 'NONE', #5099 ) ;
#4299 = CARTESIAN_POINT ( 'NONE',  ( -0.9202351150032750393, 39.19788638760600463, 92.45433879953095868 ) ) ;
#4300 = CARTESIAN_POINT ( 'NONE',  ( 29.03948732994507864, 36.35905713404685002, 74.70433879953100131 ) ) ;
#4301 = EDGE_CURVE ( 'NONE', #1145, #13369, #5102, .T. ) ;
#4302 = CARTESIAN_POINT ( 'NONE',  ( -4.007890887056452023, 40.01116025973682611, 94.04808879782397923 ) ) ;
#4303 = EDGE_CURVE ( 'NONE', #16845, #18638, #14786, .T. ) ;
#4304 = VECTOR ( 'NONE', #7118, 1000.000000000000000 ) ;
#4305 = LINE ( 'NONE', #4611, #5554 ) ;
#4306 = ADVANCED_FACE ( 'NONE', ( #207 ), #19779, .F. ) ;
#4307 = CARTESIAN_POINT ( 'NONE',  ( 5.434476177758928550, 36.85657491614816195, 76.36627918048426977 ) ) ;
#4308 = DIRECTION ( 'NONE',  ( -1.779391786395883536E-16, -5.922860397471806844E-17, 1.000000000000000000 ) ) ;
#4309 = ORIENTED_EDGE ( 'NONE', *, *, #4153, .F. ) ;
#4310 = CARTESIAN_POINT ( 'NONE',  ( 1.631982057795271501, 52.20532641826535780, 75.56770918405875648 ) ) ;
#4311 = VERTEX_POINT ( 'NONE', #1717 ) ;
#4312 = PLANE ( 'NONE',  #3391 ) ;
#4313 = CARTESIAN_POINT ( 'NONE',  ( 5.801534520520057470, 37.11886136902160160, 77.67950998295866327 ) ) ;
#4314 = CARTESIAN_POINT ( 'NONE',  ( -2.416137431568557314, 39.07291177436112406, 96.11746380123797451 ) ) ;
#4315 = ORIENTED_EDGE ( 'NONE', *, *, #10962, .F. ) ;
#4316 = AXIS2_PLACEMENT_3D ( 'NONE', #13268, #3474, #16151 ) ;
#4317 = CARTESIAN_POINT ( 'NONE',  ( -3.638656433990026695, 36.29518963458221492, 75.82994300095940332 ) ) ;
#4318 = CARTESIAN_POINT ( 'NONE',  ( 5.760694563098077481, 51.23309689197249384, 79.54845644658969661 ) ) ;
#4319 = ORIENTED_EDGE ( 'NONE', *, *, #1191, .T. ) ;
#4320 = DIRECTION ( 'NONE',  ( -0.9534635866061452747, -0.3015081906286225522, -2.009271279954815797E-16 ) ) ;
#4321 = CARTESIAN_POINT ( 'NONE',  ( 6.705715917364262424, 48.58072850854415492, 72.45432679953087529 ) ) ;
#4322 = CARTESIAN_POINT ( 'NONE',  ( 8.456021123984127641, 40.13695625074483786, 75.80967849220077426 ) ) ;
#4323 = EDGE_LOOP ( 'NONE', ( #19592, #5110 ) ) ;
#4324 = CARTESIAN_POINT ( 'NONE',  ( 6.351167193117434273, 49.92987544885872353, 75.73266097293476662 ) ) ;
#4325 = CARTESIAN_POINT ( 'NONE',  ( -7.539150955374725349, 40.44932034567779056, 79.25635544885822981 ) ) ;
#4326 = DIRECTION ( 'NONE',  ( 4.924280921909906060E-16, -1.000000000000000000, -1.532084075168673041E-30 ) ) ;
#4327 = EDGE_CURVE ( 'NONE', #5606, #10143, #6692, .T. ) ;
#4328 = CARTESIAN_POINT ( 'NONE',  ( -5.784195910403845176, 44.99242805365518194, 91.03933880123798872 ) ) ;
#4329 = PLANE ( 'NONE',  #13180 ) ;
#4330 = AXIS2_PLACEMENT_3D ( 'NONE', #5939, #3137, #17325 ) ;
#4331 = CARTESIAN_POINT ( 'NONE',  ( 5.429452001895136881, 51.47777242866884251, 75.37972891991934432 ) ) ;
#4332 = CARTESIAN_POINT ( 'NONE',  ( 3.122153740306552905, 48.66551347115873227, 93.85183880294498238 ) ) ;
#4333 = VECTOR ( 'NONE', #14643, 1000.000000000000000 ) ;
#4334 = LINE ( 'NONE', #12440, #1449 ) ;
#4335 = CARTESIAN_POINT ( 'NONE',  ( 8.372590497971586387, 41.80698495966687034, 78.77153038569251464 ) ) ;
#4336 = CARTESIAN_POINT ( 'NONE',  ( -0.9221579532582926397, 52.97975483202236546, 78.52473566685461037 ) ) ;
#4337 = EDGE_LOOP ( 'NONE', ( #2808, #8604, #2309, #12193 ) ) ;
#4338 = DIRECTION ( 'NONE',  ( -0.9485903129789527988, 0.3165065846431829311, -8.934458285744989980E-17 ) ) ;
#4339 = CARTESIAN_POINT ( 'NONE',  ( 8.661599634585135377, 45.15687757339797059, 75.45433879953088763 ) ) ;
#4340 = CARTESIAN_POINT ( 'NONE',  ( -4.274069566951154364, 51.55074801458793132, 79.52610421797659512 ) ) ;
#4341 = AXIS2_PLACEMENT_3D ( 'NONE', #18443, #12284, #2586 ) ;
#4342 = CARTESIAN_POINT ( 'NONE',  ( -8.256031663946394872, 42.72105353206794831, 79.08626245367327101 ) ) ;
#4343 = DIRECTION ( 'NONE',  ( -0.8043570849667502909, 0.5941461771852041274, -1.733862608105461749E-17 ) ) ;
#4344 = ORIENTED_EDGE ( 'NONE', *, *, #16750, .F. ) ;
#4345 = LINE ( 'NONE', #10870, #551 ) ;
#4346 = LINE ( 'NONE', #15856, #1611 ) ;
#4347 = CARTESIAN_POINT ( 'NONE',  ( 2.522153740306507519, 47.62628298661744708, 69.15433879953098995 ) ) ;
#4348 = LINE ( 'NONE', #2772, #13039 ) ;
#4349 = LINE ( 'NONE', #7664, #6358 ) ;
#4350 = FACE_OUTER_BOUND ( 'NONE', #16434, .T. ) ;
#4351 = FACE_BOUND ( 'NONE', #6204, .T. ) ;
#4352 = VECTOR ( 'NONE', #12287, 1000.000000000000114 ) ;
#4353 = VERTEX_POINT ( 'NONE', #10017 ) ;
#4354 = CARTESIAN_POINT ( 'NONE',  ( -5.784195910403845176, 44.99242805365518194, 92.13308880123798872 ) ) ;
#4355 = EDGE_CURVE ( 'NONE', #18944, #3817, #16496, .T. ) ;
#4356 = CARTESIAN_POINT ( 'NONE',  ( -7.677846259693480668, 44.16218137147969003, 56.15433879953099705 ) ) ;
#4357 = ORIENTED_EDGE ( 'NONE', *, *, #12972, .F. ) ;
#4358 = CARTESIAN_POINT ( 'NONE',  ( 5.512699119566887518, 50.66164519424028612, 77.25083512729199242 ) ) ;
#4359 = VERTEX_POINT ( 'NONE', #5199 ) ;
#4360 = CARTESIAN_POINT ( 'NONE',  ( -5.590960105440975880, 48.67769231808699715, 72.45432679953087529 ) ) ;
#4361 = APPLICATION_CONTEXT ( 'automotive_design' ) ;
#4362 = CARTESIAN_POINT ( 'NONE',  ( 5.025485839985549319, 41.56218137147963887, 91.03933880294498238 ) ) ;
#4363 = EDGE_LOOP ( 'NONE', ( #15598, #13789, #4891, #16765, #6511, #6968, #9812, #11787 ) ) ;
#4364 = DIRECTION ( 'NONE',  ( 1.621236893436268647E-16, 2.273814620809075225E-32, -1.000000000000000000 ) ) ;
#4365 = AXIS2_PLACEMENT_3D ( 'NONE', #3434, #8336, #14918 ) ;
#4366 = ADVANCED_FACE ( 'NONE', ( #11719 ), #20415, .T. ) ;
#4367 = CARTESIAN_POINT ( 'NONE',  ( 0.5221537403065019678, 51.36218137147968577, 87.21440135111343750 ) ) ;
#4368 = LINE ( 'NONE', #12683, #994 ) ;
#4369 = CARTESIAN_POINT ( 'NONE',  ( 30.92220646078100188, 36.96218137147968008, 29.55715055817103476 ) ) ;
#4370 = CARTESIAN_POINT ( 'NONE',  ( 0.8408802816388469825, 52.35219974923202102, 76.19252767286178596 ) ) ;
#4371 = LINE ( 'NONE', #10897, #10637 ) ;
#4372 = VERTEX_POINT ( 'NONE', #10665 ) ;
#4373 = LINE ( 'NONE', #6077, #7468 ) ;
#4374 = CARTESIAN_POINT ( 'NONE',  ( -4.622577041588896485, 46.56120873422322859, 93.65746379782397923 ) ) ;
#4375 = EDGE_LOOP ( 'NONE', ( #12959, #17072, #7176, #1825 ) ) ;
#4376 = LINE ( 'NONE', #4272, #13159 ) ;
#4377 = PLANE ( 'NONE',  #10494 ) ;
#4378 = CARTESIAN_POINT ( 'NONE',  ( 1.352400422481993658, 50.46853102219002096, 95.57058880123798872 ) ) ;
#4379 = CARTESIAN_POINT ( 'NONE',  ( -7.507604988220667686, 45.82440120099734315, 79.45433879953087342 ) ) ;
#4380 = CARTESIAN_POINT ( 'NONE',  ( 5.848951923618479931, 37.15274410921379911, 76.58742703482498371 ) ) ;
#4381 = CARTESIAN_POINT ( 'NONE',  ( 6.388020695587198539, 49.89220557922158861, 79.05872268769354605 ) ) ;
#4382 = VECTOR ( 'NONE', #15749, 1000.000000000000000 ) ;
#4383 = EDGE_LOOP ( 'NONE', ( #17540, #1940, #20503, #543, #18171, #19708 ) ) ;
#4384 = CARTESIAN_POINT ( 'NONE',  ( 4.609531566588798590, 52.08341462581984871, 78.11943565213420015 ) ) ;
#4385 = VERTEX_POINT ( 'NONE', #10447 ) ;
#4386 = VECTOR ( 'NONE', #10167, 1000.000000000000000 ) ;
#4387 = CARTESIAN_POINT ( 'NONE',  ( -3.373440834332912086, 52.19430433279444514, 76.25796290525131838 ) ) ;
#4388 = CARTESIAN_POINT ( 'NONE',  ( -4.567115856812060670, 47.10047254335474065, 94.71121380123797451 ) ) ;
#4389 = CARTESIAN_POINT ( 'NONE',  ( -1.219056181852248066, 49.77488197367201650, 94.56237966814981633 ) ) ;
#4390 = ORIENTED_EDGE ( 'NONE', *, *, #11294, .T. ) ;
#4391 = VECTOR ( 'NONE', #20805, 1000.000000000000114 ) ;
#4392 = CARTESIAN_POINT ( 'NONE',  ( -5.000220527482744259, 50.11192012471359192, 79.30596685730465367 ) ) ;
#4393 = LINE ( 'NONE', #17388, #17756 ) ;
#4394 = VERTEX_POINT ( 'NONE', #18721 ) ;
#4395 = CARTESIAN_POINT ( 'NONE',  ( 6.046986631774924348, 37.29425246114896453, 78.37121987722640881 ) ) ;
#4396 = EDGE_CURVE ( 'NONE', #2580, #19160, #10342, .T. ) ;
#4397 = CARTESIAN_POINT ( 'NONE',  ( -4.598246518171406727, 51.31910303412165320, 78.93669174070734584 ) ) ;
#4398 = ORIENTED_EDGE ( 'NONE', *, *, #5211, .F. ) ;
#4399 = CARTESIAN_POINT ( 'NONE',  ( -1.883296302981686043, 36.95289499283964574, 75.45433879953087342 ) ) ;
#4400 = VECTOR ( 'NONE', #18717, 1000.000000000000000 ) ;
#4401 = LINE ( 'NONE', #15705, #6220 ) ;
#4402 = EDGE_CURVE ( 'NONE', #20886, #14909, #11256, .T. ) ;
#4403 = VERTEX_POINT ( 'NONE', #4026 ) ;
#4404 = DIRECTION ( 'NONE',  ( 0.9999689119394085113, -0.007885122365275719011, 1.526048693634352652E-16 ) ) ;
#4405 = CARTESIAN_POINT ( 'NONE',  ( 5.596449423573146120, 45.91824161709900665, 95.05433879953102405 ) ) ;
#4406 = CARTESIAN_POINT ( 'NONE',  ( -4.622577041588895597, 46.56120873422322859, 91.31371379782397923 ) ) ;
#4407 = CIRCLE ( 'NONE', #8847, 8.199999999999995737 ) ;
#4408 = CARTESIAN_POINT ( 'NONE',  ( -3.936224163802635179, 36.51499092983547001, 77.70026928173652436 ) ) ;
#4409 = VECTOR ( 'NONE', #8481, 999.9999999999998863 ) ;
#4411 = EDGE_CURVE ( 'NONE', #5376, #1084, #7331, .T. ) ;
#4410 = CARTESIAN_POINT ( 'NONE',  ( 8.801580714196775901, 41.17262026450377022, 76.07953452682116335 ) ) ;
#4412 = EDGE_CURVE ( 'NONE', #12733, #13051, #20089, .T. ) ;
#4413 = CARTESIAN_POINT ( 'NONE',  ( -3.936408902674057853, 36.51512738899804589, 77.68304435440727218 ) ) ;
#4414 = EDGE_CURVE ( 'NONE', #17910, #14291, #3711, .T. ) ;
#4415 = EDGE_LOOP ( 'NONE', ( #16356, #2524, #9337, #6805, #12005 ) ) ;
#4416 = LINE ( 'NONE', #14522, #19336 ) ;
#4417 = VECTOR ( 'NONE', #9984, 1000.000000000000000 ) ;
#4418 = AXIS2_PLACEMENT_3D ( 'NONE', #4080, #15480, #7493 ) ;
#4419 = PRODUCT_RELATED_PRODUCT_CATEGORY ( 'part', '', ( #3597 ) ) ;
#4420 = ORIENTED_EDGE ( 'NONE', *, *, #16540, .T. ) ;
#4421 = DIRECTION ( 'NONE',  ( 1.110223024625156540E-16, 1.000000000000000000, 5.922860397471808077E-17 ) ) ;
#4422 = EDGE_CURVE ( 'NONE', #10826, #10346, #7088, .T. ) ;
#4423 = CARTESIAN_POINT ( 'NONE',  ( 0.5934291639749685876, 52.36187159818830850, 75.36022115247205022 ) ) ;
#4424 = CARTESIAN_POINT ( 'NONE',  ( -2.416137431568557314, 39.07291177436112406, 94.86746380123797451 ) ) ;
#4425 = EDGE_CURVE ( 'NONE', #15803, #5518, #11239, .T. ) ;
#4426 = B_SPLINE_SURFACE_WITH_KNOTS ( 'NONE', 3, 1, ( 
 ( #5543, #7345 ),
 ( #15342, #13837 ),
 ( #8960, #5640 ),
 ( #12259, #967 ),
 ( #14933, #17039 ),
 ( #13242, #14831 ),
 ( #10777, #13737 ),
 ( #4252, #20105 ),
 ( #7129, #756 ),
 ( #18135, #20208 ),
 ( #16929, #1961 ),
 ( #12149, #2352 ),
 ( #18738, #17143 ),
 ( #6736, #861 ),
 ( #18630, #357 ),
 ( #19721, #13630 ),
 ( #18526, #3939 ),
 ( #8854, #16541 ),
 ( #12365, #10464 ),
 ( #3556, #8453 ),
 ( #2465, #2564 ),
 ( #20316, #10060 ),
 ( #7242, #13952 ) ),
 .UNSPECIFIED., .F., .F., .F.,
 ( 4, 1, 1, 1, 1, 1, 1, 1, 1, 1, 1, 1, 1, 1, 1, 1, 1, 1, 1, 1, 4 ),
 ( 2, 2 ),
 ( 0.000000000000000000, 0.08067270264552857395, 0.1526829783898679127, 0.2165906325091179196, 0.2718813074182493406, 0.3185216544617175960, 0.3571485182974105665, 0.3872397186037628281, 0.4089098634073701777, 0.4447579376399536377, 0.4819898389264800631, 0.5235943582205320190, 0.5710910199931596987, 0.5998727328596447084, 0.6352309269333883401, 0.6779581688328760736, 0.7280061531568029487, 0.7849809541712158278, 0.8494662260529197706, 0.9209515060471785697, 0.9999999999999998890 ),
 ( 0.000000000000000000, 1.000000000000000000 ),
 .UNSPECIFIED. ) ;
#4427 = CARTESIAN_POINT ( 'NONE',  ( -3.236474689574856622, 51.45049332321921298, 75.68338214653230978 ) ) ;
#4428 = EDGE_LOOP ( 'NONE', ( #15907, #6305, #11848, #1756 ) ) ;
#4429 = EDGE_LOOP ( 'NONE', ( #13041, #2045, #3043, #12420 ) ) ;
#4430 = VECTOR ( 'NONE', #9803, 1000.000000000000227 ) ;
#4431 = CARTESIAN_POINT ( 'NONE',  ( -3.522342774269683563, 36.20927341954680401, 76.21065298426071877 ) ) ;
#4432 = CARTESIAN_POINT ( 'NONE',  ( -6.951684312017277989, 40.78766315881389204, 77.34121496451329847 ) ) ;
#4433 = ORIENTED_EDGE ( 'NONE', *, *, #5438, .T. ) ;
#4434 = EDGE_CURVE ( 'NONE', #20845, #14379, #8389, .T. ) ;
#4435 = DIRECTION ( 'NONE',  ( -1.571217453038212812E-16, -0.7071067811865500152, -0.7071067811865451302 ) ) ;
#4436 = DIRECTION ( 'NONE',  ( 1.540237394707284220E-16, 1.793354297423764243E-16, -1.000000000000000000 ) ) ;
#4437 = CARTESIAN_POINT ( 'NONE',  ( 8.385679600361122255, 39.92613824206362949, 77.13595644658970230 ) ) ;
#4438 = EDGE_LOOP ( 'NONE', ( #14208, #5596, #117, #16232, #13575, #1535, #19184, #491 ) ) ;
#4439 = CARTESIAN_POINT ( 'NONE',  ( -5.072433652944413396, 37.35426311015447709, 77.90218689189877921 ) ) ;
#4440 = CARTESIAN_POINT ( 'NONE',  ( -7.420489402526318834, 40.07407525022878048, 78.61740305894309699 ) ) ;
#4441 = CARTESIAN_POINT ( 'NONE',  ( 1.964251312053307830, 36.08998497932209659, 75.45433879953088763 ) ) ;
#4442 = CARTESIAN_POINT ( 'NONE',  ( 1.352400422481993658, 50.46853102219002096, 95.57058880123798872 ) ) ;
#4443 = LINE ( 'NONE', #4226, #10818 ) ;
#4444 = CARTESIAN_POINT ( 'NONE',  ( 8.484205517248936346, 46.29100619283276785, 79.46269805960562849 ) ) ;
#4445 = LINE ( 'NONE', #10961, #17743 ) ;
#4446 = SURFACE_STYLE_USAGE ( .BOTH. , #17331 ) ;
#4447 = CARTESIAN_POINT ( 'NONE',  ( 31.03948732994507864, 43.16218137147969003, 76.90433879953100416 ) ) ;
#4448 = PLANE ( 'NONE',  #4472 ) ;
#4449 = ADVANCED_FACE ( 'NONE', ( #3823 ), #5627, .T. ) ;
#4450 = LINE ( 'NONE', #6459, #18062 ) ;
#4451 = ORIENTED_EDGE ( 'NONE', *, *, #14847, .T. ) ;
#4452 = CARTESIAN_POINT ( 'NONE',  ( 5.722153740306817227, 44.84677435893293307, 94.60825776475003579 ) ) ;
#4453 = CARTESIAN_POINT ( 'NONE',  ( 5.760549983993971779, 37.08957531975971023, 75.99604373986946371 ) ) ;
#4454 = ORIENTED_EDGE ( 'NONE', *, *, #603, .T. ) ;
#4455 = CARTESIAN_POINT ( 'NONE',  ( 8.214904837957266892, 41.32288909301291113, 78.51180775816763457 ) ) ;
#4456 = CARTESIAN_POINT ( 'NONE',  ( -3.597291554029903526, 36.26463506403467107, 78.92082147625116306 ) ) ;
#4457 = LINE ( 'NONE', #3284, #19113 ) ;
#4458 = DIRECTION ( 'NONE',  ( -1.540237394707284220E-16, -1.793354297423764243E-16, 1.000000000000000000 ) ) ;
#4459 = DIRECTION ( 'NONE',  ( -0.7071067811865474617, 1.203855704449244074E-16, -0.7071067811865476838 ) ) ;
#4460 = VECTOR ( 'NONE', #18003, 1000.000000000000114 ) ;
#4461 = CARTESIAN_POINT ( 'NONE',  ( -4.062845822180057631, 50.96055957082182175, 78.82314076797449331 ) ) ;
#4462 = CARTESIAN_POINT ( 'NONE',  ( 31.03948732994507864, 36.35905713404685002, 76.90433879953100416 ) ) ;
#4463 = PLANE ( 'NONE',  #13389 ) ;
#4464 = VECTOR ( 'NONE', #15325, 1000.000000000000000 ) ;
#4465 = ORIENTED_EDGE ( 'NONE', *, *, #10411, .T. ) ;
#4466 = CARTESIAN_POINT ( 'NONE',  ( -5.940171601930143375, 37.99522617845349970, 78.80728580974474085 ) ) ;
#4467 = CARTESIAN_POINT ( 'NONE',  ( -5.052695833059940078, 50.99437019215367428, 79.48628414162533318 ) ) ;
#4468 = CARTESIAN_POINT ( 'NONE',  ( 5.981342461385748877, 37.24734554037533485, 78.37107466246847309 ) ) ;
#4469 = VERTEX_POINT ( 'NONE', #16035 ) ;
#4470 = AXIS2_PLACEMENT_3D ( 'NONE', #14388, #12897, #20861 ) ;
#4471 = LINE ( 'NONE', #17663, #12266 ) ;
#4472 = AXIS2_PLACEMENT_3D ( 'NONE', #7436, #6044, #10967 ) ;
#4473 = CARTESIAN_POINT ( 'NONE',  ( 1.868012774839550749, 39.13936707477651566, 92.13308880294498238 ) ) ;
#4474 = ORIENTED_EDGE ( 'NONE', *, *, #3868, .T. ) ;
#4475 = LINE ( 'NONE', #19550, #11682 ) ;
#4476 = LINE ( 'NONE', #2678, #8454 ) ;
#4477 = CARTESIAN_POINT ( 'NONE',  ( 5.455102971993217587, 51.45882509034149166, 79.53290755650829169 ) ) ;
#4478 = CARTESIAN_POINT ( 'NONE',  ( -5.510796958474740492, 38.60848837797752964, 78.53742703482498655 ) ) ;
#4479 = FACE_BOUND ( 'NONE', #18657, .T. ) ;
#4480 = CARTESIAN_POINT ( 'NONE',  ( -3.798798875594518787, 36.41348040526440144, 79.26586447293077242 ) ) ;
#4481 = ORIENTED_EDGE ( 'NONE', *, *, #5592, .F. ) ;
#4482 = LINE ( 'NONE', #9608, #1019 ) ;
#4483 = CARTESIAN_POINT ( 'NONE',  ( -4.622577041588896485, 46.56120873422322859, 92.40746379782397923 ) ) ;
#4484 = EDGE_LOOP ( 'NONE', ( #7351, #8363, #20767, #20462 ) ) ;
#4485 = CARTESIAN_POINT ( 'NONE',  ( 6.705715917364262424, 48.58072850854415492, 72.45433879953087342 ) ) ;
#4486 = CARTESIAN_POINT ( 'NONE',  ( -5.154188915835984375, 42.64120994080404614, 94.71121380123797451 ) ) ;
#4487 = CARTESIAN_POINT ( 'NONE',  ( -5.955451856753747109, 38.00651308716548726, 76.73301527011911105 ) ) ;
#4488 = AXIS2_PLACEMENT_3D ( 'NONE', #7516, #13891, #15607 ) ;
#4489 = CARTESIAN_POINT ( 'NONE',  ( -6.360298161978083620, 42.04670741611674600, 79.54845644658969661 ) ) ;
#4490 = CARTESIAN_POINT ( 'NONE',  ( -7.350415620663316218, 41.88927500876809518, 78.85747680284711691 ) ) ;
#4491 = VECTOR ( 'NONE', #17233, 1000.000000000000227 ) ;
#4492 = EDGE_LOOP ( 'NONE', ( #11743, #2735, #13617, #14146, #14525, #3316 ) ) ;
#4493 = DIRECTION ( 'NONE',  ( -1.084202172485505420E-16, -1.000000000000000000, 0.000000000000000000 ) ) ;
#4494 = ORIENTED_EDGE ( 'NONE', *, *, #13092, .F. ) ;
#4495 = CARTESIAN_POINT ( 'NONE',  ( -3.496280357775573222, 52.10652770678432688, 75.88277413867518817 ) ) ;
#4496 = CARTESIAN_POINT ( 'NONE',  ( 2.043125170982144745, 38.48583871533720213, 92.67996380123798872 ) ) ;
#4497 = CARTESIAN_POINT ( 'NONE',  ( 10.77494014480653917, 42.96218137147968008, 58.20715055817105110 ) ) ;
#4498 = ORIENTED_EDGE ( 'NONE', *, *, #15944, .T. ) ;
#4499 = CARTESIAN_POINT ( 'NONE',  ( 4.004906909697989015, 36.73854140438177041, 77.43080938776617472 ) ) ;
#4500 = AXIS2_PLACEMENT_3D ( 'NONE', #17903, #9831, #8334 ) ;
#4501 = CARTESIAN_POINT ( 'NONE',  ( 0.5221537403065188432, 44.16218137147969003, 54.55433879953099563 ) ) ;
#4502 = B_SPLINE_CURVE_WITH_KNOTS ( 'NONE', 3,
 ( #10676, #6057, #15767, #2561, #20530, #4461, #12557, #17349, #12455, #18936, #15860, #4246 ),
 .UNSPECIFIED., .F., .F.,
 ( 4, 2, 2, 2, 2, 4 ),
 ( 0.000000000000000000, 0.0001618041688235931916, 0.0002427062532353941649, 0.0003236083376471951653, 0.0004854125064707999850, 0.0006472166752944048590 ),
 .UNSPECIFIED. ) ;
#4503 = CARTESIAN_POINT ( 'NONE',  ( 5.563409226749892689, 51.37882362279480475, 76.27120023672567584 ) ) ;
#4504 = AXIS2_PLACEMENT_3D ( 'NONE', #10364, #15028, #444 ) ;
#4505 = ADVANCED_FACE ( 'NONE', ( #16140 ), #6431, .T. ) ;
#4506 = ORIENTED_EDGE ( 'NONE', *, *, #1024, .T. ) ;
#4507 = LINE ( 'NONE', #4399, #6794 ) ;
#4508 = CARTESIAN_POINT ( 'NONE',  ( 6.828503391016846891, 43.33193468930419101, 91.66433880123796030 ) ) ;
#4509 = ORIENTED_EDGE ( 'NONE', *, *, #2570, .T. ) ;
#4510 = CARTESIAN_POINT ( 'NONE',  ( -5.246808833622705670, 49.98991590973655263, 79.09052234626923905 ) ) ;
#4511 = CARTESIAN_POINT ( 'NONE',  ( 5.200945329014118990, 40.92307955209284387, 95.05433879953095300 ) ) ;
#4512 = CARTESIAN_POINT ( 'NONE',  ( 2.463659247115865369, 38.82793883177424732, 95.53246379782397923 ) ) ;
#4513 = CARTESIAN_POINT ( 'NONE',  ( 5.549530740019891439, 36.93878869392346331, 75.99415254657458263 ) ) ;
#4514 = CARTESIAN_POINT ( 'NONE',  ( 8.787842894572216679, 41.13144714757795128, 76.38644048143638088 ) ) ;
#4515 = VECTOR ( 'NONE', #3832, 1000.000000000000000 ) ;
#4516 = LINE ( 'NONE', #9017, #20107 ) ;
#4517 = ADVANCED_FACE ( 'NONE', ( #6326 ), #18829, .T. ) ;
#4518 = ORIENTED_EDGE ( 'NONE', *, *, #7260, .T. ) ;
#4519 = DIRECTION ( 'NONE',  ( -0.9585804129707224952, -0.2848220354341972071, -1.987228219138359305E-16 ) ) ;
#4520 = B_SPLINE_CURVE_WITH_KNOTS ( 'NONE', 3,
 ( #9294, #15783, #9186, #17566, #7682, #2989, #3100, #14159, #20642, #6072 ),
 .UNSPECIFIED., .F., .F.,
 ( 4, 2, 2, 2, 4 ),
 ( 0.000000000000000000, 0.0001564258200695812736, 0.0002346387301043621797, 0.0003128516401391430858, 0.0006257032802783057956 ),
 .UNSPECIFIED. ) ;
#4521 = ORIENTED_EDGE ( 'NONE', *, *, #9457, .F. ) ;
#4522 = CARTESIAN_POINT ( 'NONE',  ( -7.962931747100077118, 41.82371769612938550, 77.49347059784275871 ) ) ;
#4523 = LINE ( 'NONE', #11040, #12978 ) ;
#4524 = CARTESIAN_POINT ( 'NONE',  ( 5.611423337425062385, 41.22389019960463230, 92.83621380123797451 ) ) ;
#4525 = EDGE_CURVE ( 'NONE', #15383, #15567, #1349, .T. ) ;
#4526 = CARTESIAN_POINT ( 'NONE',  ( 2.108290839596759447, 51.34989793853182505, 76.48963291717792856 ) ) ;
#4527 = VERTEX_POINT ( 'NONE', #14636 ) ;
#4528 = VERTEX_POINT ( 'NONE', #17724 ) ;
#4529 = CARTESIAN_POINT ( 'NONE',  ( -3.232751207032058094, 36.92019674127485729, 75.77010869825431882 ) ) ;
#4530 = CARTESIAN_POINT ( 'NONE',  ( 8.378694375505322256, 41.81382678022286115, 78.47674047826052401 ) ) ;
#4531 = CARTESIAN_POINT ( 'NONE',  ( 5.716051675127889808, 50.35205778976271773, 79.51305506302354331 ) ) ;
#4532 = VERTEX_POINT ( 'NONE', #19309 ) ;
#4533 = CARTESIAN_POINT ( 'NONE',  ( 4.141216478295206116, 51.51532511143173565, 78.50413411530853125 ) ) ;
#4534 = EDGE_CURVE ( 'NONE', #11768, #6129, #3157, .T. ) ;
#4535 = CARTESIAN_POINT ( 'NONE',  ( -6.709242558049761662, 40.29605830358345031, 78.50801527011910252 ) ) ;
#4536 = CARTESIAN_POINT ( 'NONE',  ( 7.700557761655851152, 40.25396938766707677, 76.00709785348774972 ) ) ;
#4537 = EDGE_CURVE ( 'NONE', #13701, #1203, #463, .T. ) ;
#4538 = CIRCLE ( 'NONE', #15770, 4.199999999999999289 ) ;
#4539 = ORIENTED_EDGE ( 'NONE', *, *, #6835, .T. ) ;
#4540 = DIRECTION ( 'NONE',  ( -1.193617070626243484E-16, -1.000000000000000000, -0.000000000000000000 ) ) ;
#4541 = CARTESIAN_POINT ( 'NONE',  ( 5.902048492000326441, 51.12868443877599134, 78.27786821129558348 ) ) ;
#4542 = FACE_OUTER_BOUND ( 'NONE', #13893, .T. ) ;
#4543 = CARTESIAN_POINT ( 'NONE',  ( -0.3080929418689875576, 37.85583172076933778, 93.85183880123797451 ) ) ;
#4544 =( LENGTH_UNIT ( ) NAMED_UNIT ( * ) SI_UNIT ( .MILLI., .METRE. ) );
#4545 = ADVANCED_FACE ( 'NONE', ( #7840 ), #11460, .T. ) ;
#4546 = CARTESIAN_POINT ( 'NONE',  ( 5.544968037009670780, 45.50804040601273925, 89.94558880294498238 ) ) ;
#4547 = LINE ( 'NONE', #20710, #14008 ) ;
#4548 = FACE_OUTER_BOUND ( 'NONE', #5380, .T. ) ;
#4549 = CARTESIAN_POINT ( 'NONE',  ( -0.3473626758238653744, 52.97522236001905327, 79.37504392981026058 ) ) ;
#4550 = CARTESIAN_POINT ( 'NONE',  ( 0.3279640439667345642, 52.35988168082470651, 77.76169174070734869 ) ) ;
#4551 = CARTESIAN_POINT ( 'NONE',  ( 11.22215374030649926, 42.76218137147968434, 70.80574467885102763 ) ) ;
#4552 = DIRECTION ( 'NONE',  ( 0.007885122365275663500, 0.9999689119394085113, 1.805443505845543142E-16 ) ) ;
#4553 = CARTESIAN_POINT ( 'NONE',  ( 3.460444912181559474, 49.25145096859824889, 91.89871380123798872 ) ) ;
#4554 = VERTEX_POINT ( 'NONE', #9862 ) ;
#4555 = CARTESIAN_POINT ( 'NONE',  ( 2.447781712115294273, 38.42313889284341144, 72.45432679953087529 ) ) ;
#4557 = EDGE_CURVE ( 'NONE', #6157, #867, #10170, .T. ) ;
#4556 = CARTESIAN_POINT ( 'NONE',  ( -4.677846259693498432, 44.16218137147969003, 92.70661078214052964 ) ) ;
#4558 = CARTESIAN_POINT ( 'NONE',  ( 5.155652520773657876, 37.39667442584504897, 77.72325690743420523 ) ) ;
#4559 = CARTESIAN_POINT ( 'NONE',  ( -5.004817973257477348, 39.29348442311233214, 76.73301527011911105 ) ) ;
#4560 = CARTESIAN_POINT ( 'NONE',  ( 5.245694785492322154, 50.86039100563218085, 78.13212606300182017 ) ) ;
#4561 = CARTESIAN_POINT ( 'NONE',  ( 6.507463592229761673, 49.75665574485773135, 76.97234655072247733 ) ) ;
#4562 = DIRECTION ( 'NONE',  ( 0.000000000000000000, 0.000000000000000000, 1.000000000000000000 ) ) ;
#4563 = EDGE_CURVE ( 'NONE', #18617, #10971, #16345, .T. ) ;
#4564 = EDGE_CURVE ( 'NONE', #9068, #19085, #16667, .T. ) ;
#4565 = ADVANCED_FACE ( 'NONE', ( #3255 ), #163, .F. ) ;
#4566 = CARTESIAN_POINT ( 'NONE',  ( -5.075010979219785057, 38.29217337334619486, 79.43312132436682305 ) ) ;
#4567 = DIRECTION ( 'NONE',  ( 0.2999031954727301441, 0.9539696396349547358, 2.172727669310452375E-16 ) ) ;
#4568 = CARTESIAN_POINT ( 'NONE',  ( 5.332873941910801108, 50.80275800021833277, 78.92693817761565356 ) ) ;
#4569 = ORIENTED_EDGE ( 'NONE', *, *, #12563, .T. ) ;
#4570 = CARTESIAN_POINT ( 'NONE',  ( 23.03948732994508575, 43.16218137147969003, 76.90433879953101837 ) ) ;
#4571 = CARTESIAN_POINT ( 'NONE',  ( 3.122153740306552905, 48.66551347115873227, 93.85183880294498238 ) ) ;
#4572 = ORIENTED_EDGE ( 'NONE', *, *, #2635, .T. ) ;
#4573 = CARTESIAN_POINT ( 'NONE',  ( -6.613032277150673544, 45.52591812603678534, 75.45433879953087342 ) ) ;
#4574 = DIRECTION ( 'NONE',  ( 0.3165065846431827645, 0.9485903129789529098, 0.000000000000000000 ) ) ;
#4575 = CARTESIAN_POINT ( 'NONE',  ( 4.199109002476567376, 47.83913663364971569, 93.48786078214052964 ) ) ;
#4576 = CARTESIAN_POINT ( 'NONE',  ( -5.405939962049822078, 49.82766502745145942, 76.76022115247205591 ) ) ;
#4577 = CARTESIAN_POINT ( 'NONE',  ( 0.5221537403065079630, 49.16218137147969003, 93.97886871425482980 ) ) ;
#4578 = CARTESIAN_POINT ( 'NONE',  ( -1.211118738164628672, 49.47529140343971221, 92.45433879953100131 ) ) ;
#4579 = VERTEX_POINT ( 'NONE', #262 ) ;
#4580 = DIRECTION ( 'NONE',  ( 1.540237394707284220E-16, 1.793354297423764243E-16, -1.000000000000000000 ) ) ;
#4581 = VERTEX_POINT ( 'NONE', #5044 ) ;
#4582 = DIRECTION ( 'NONE',  ( -1.000000000000000000, 4.818676322157797375E-16, 0.000000000000000000 ) ) ;
#4583 = EDGE_CURVE ( 'NONE', #1468, #18137, #5252, .T. ) ;
#4584 = CARTESIAN_POINT ( 'NONE',  ( 1.087774996680691109, 52.94836625043949851, 76.77198585835439815 ) ) ;
#4585 = CARTESIAN_POINT ( 'NONE',  ( -4.792503378000012582, 37.91763016944491227, 77.90139762306027649 ) ) ;
#4586 = DIRECTION ( 'NONE',  ( 0.7071067811865539010, -3.662367542345418158E-17, -0.7071067811865411334 ) ) ;
#4587 = B_SPLINE_SURFACE_WITH_KNOTS ( 'NONE', 3, 1, ( 
 ( #4098, #17096 ),
 ( #12617, #17196 ),
 ( #14202, #20485 ),
 ( #19104, #9016 ),
 ( #12201, #10627 ),
 ( #14002, #17402 ),
 ( #15818, #1022 ),
 ( #12512, #15501 ),
 ( #5807, #20679 ),
 ( #18793, #18680 ),
 ( #12313, #2520 ) ),
 .UNSPECIFIED., .F., .F., .F.,
 ( 4, 1, 1, 1, 1, 1, 1, 1, 4 ),
 ( 2, 2 ),
 ( 0.000000000000000000, 0.2096989846417539882, 0.3830033715279665407, 0.5180517223345033617, 0.6192761841629320640, 0.7029005363942016915, 0.7892332632667665715, 0.8867012962659018838, 1.000000000000000000 ),
 ( 0.000000000000000000, 1.000000000000000000 ),
 .UNSPECIFIED. ) ;
#4588 = EDGE_LOOP ( 'NONE', ( #2849, #15139 ) ) ;
#4589 = CARTESIAN_POINT ( 'NONE',  ( 9.353187571392870936, 42.82582100880699016, 77.22643688620827618 ) ) ;
#4590 = ORIENTED_EDGE ( 'NONE', *, *, #12438, .F. ) ;
#4591 = CARTESIAN_POINT ( 'NONE',  ( 5.037341483232629535, 37.31725042616477594, 78.09625056423675460 ) ) ;
#4592 = CARTESIAN_POINT ( 'NONE',  ( -4.524181921268124462, 40.28999182795290324, 92.44558880123798872 ) ) ;
#4593 = CARTESIAN_POINT ( 'NONE',  ( 4.942331607238935831, 51.83758864179496584, 75.54250430092201896 ) ) ;
#4594 = ORIENTED_EDGE ( 'NONE', *, *, #14448, .F. ) ;
#4595 = CARTESIAN_POINT ( 'NONE',  ( -5.391925874121969109, 49.83202182525327117, 78.49957729094111869 ) ) ;
#4596 = CARTESIAN_POINT ( 'NONE',  ( 2.484494565094233831, 50.04344131194918788, 78.25433879953088478 ) ) ;
#4597 = ORIENTED_EDGE ( 'NONE', *, *, #13910, .T. ) ;
#4598 = CARTESIAN_POINT ( 'NONE',  ( 4.490969506678155199, 36.18237959297783135, 75.97723610431854979 ) ) ;
#4599 = EDGE_CURVE ( 'NONE', #18313, #6954, #11982, .T. ) ;
#4600 = CARTESIAN_POINT ( 'NONE',  ( 5.694198211105373275, 51.28221506855305734, 75.97344461144770378 ) ) ;
#4601 = CARTESIAN_POINT ( 'NONE',  ( 5.428124502387796646, 36.85203624147762724, 77.45531005930804724 ) ) ;
#4602 = VERTEX_POINT ( 'NONE', #474 ) ;
#4603 = CARTESIAN_POINT ( 'NONE',  ( -4.531920369308549468, 45.91945145313098209, 92.55433879953098142 ) ) ;
#4604 = CARTESIAN_POINT ( 'NONE',  ( 5.146040402138061687, 40.41782331071202350, 90.30634062920465510 ) ) ;
#4605 = MANIFOLD_SOLID_BREP ( 'Stock-MAS-160-1', #1710 ) ;
#4606 = EDGE_LOOP ( 'NONE', ( #12672, #15087, #12277, #10657 ) ) ;
#4607 = CARTESIAN_POINT ( 'NONE',  ( 4.551159079667362661, 51.21251702529338701, 77.70137231118654597 ) ) ;
#4608 = CARTESIAN_POINT ( 'NONE',  ( 5.176717291127333809, 46.72077138471917834, 95.05433879953092458 ) ) ;
#4609 = LINE ( 'NONE', #20881, #10547 ) ;
#4610 = CARTESIAN_POINT ( 'NONE',  ( 5.666884522201894647, 41.76315400873614436, 94.43871379782397923 ) ) ;
#4611 = CARTESIAN_POINT ( 'NONE',  ( 10.77494014480653561, 42.76218137147968434, 77.40433879953098995 ) ) ;
#4612 = CARTESIAN_POINT ( 'NONE',  ( -4.340948238162491535, 40.55733868359232730, 75.45433879953087342 ) ) ;
#4613 = CARTESIAN_POINT ( 'NONE',  ( -3.557428649121372022, 36.23518994195449494, 77.32142682847380399 ) ) ;
#4614 = VERTEX_POINT ( 'NONE', #6952 ) ;
#4615 = CARTESIAN_POINT ( 'NONE',  ( 2.091073016766569648, 52.20170728465966903, 78.67719617274387645 ) ) ;
#4616 =( BOUNDED_CURVE ( )  B_SPLINE_CURVE ( 2, ( #8203, #4993, #6592, #14791, #17878, #314, #16501, #6379, #4780, #9808, #212 ),
 .UNSPECIFIED., .F., .F. ) 
 B_SPLINE_CURVE_WITH_KNOTS ( ( 3, 2, 2, 2, 2, 3 ),
 ( 0.5173390146554853741, 0.5312500000000000000, 0.5625000000000000000, 0.5937500000000000000, 0.6250000000000000000, 0.6423390146554854852 ),
 .UNSPECIFIED. ) 
 CURVE ( )  GEOMETRIC_REPRESENTATION_ITEM ( )  RATIONAL_B_SPLINE_CURVE ( ( 0.9623977609649205789, 0.9661148573551010532, 1.000000000000000000, 0.9238795325112867385, 1.000000000000000000, 0.9238795325112867385, 1.000000000000000000, 0.9238795325112867385, 1.000000000000000000, 0.9577646751561854632, 0.9623977609649205789 ) ) 
 REPRESENTATION_ITEM ( '' )  );
#4617 = EDGE_CURVE ( 'NONE', #16250, #17122, #7057, .T. ) ;
#4618 = VERTEX_POINT ( 'NONE', #18146 ) ;
#4619 = CARTESIAN_POINT ( 'NONE',  ( -7.774959294756113692, 41.22996117453095621, 78.61536821129558916 ) ) ;
#4620 = CARTESIAN_POINT ( 'NONE',  ( -0.9425155279038999190, 52.23031283747450004, 76.97503235252658271 ) ) ;
#4621 = LINE ( 'NONE', #1773, #17730 ) ;
#4622 = CARTESIAN_POINT ( 'NONE',  ( -2.920505538251614297, 51.60450474689833555, 76.49565832826704082 ) ) ;
#4623 = EDGE_LOOP ( 'NONE', ( #7614, #19859, #10727, #6571 ) ) ;
#4624 = CARTESIAN_POINT ( 'NONE',  ( 5.613949991644618720, 51.34149119567325670, 78.06835901908682729 ) ) ;
#4625 = ORIENTED_EDGE ( 'NONE', *, *, #1213, .F. ) ;
#4626 = CARTESIAN_POINT ( 'NONE',  ( -3.872497565881518611, 36.46791865901509055, 75.57130654555172100 ) ) ;
#4627 = CARTESIAN_POINT ( 'NONE',  ( 8.832380548758539618, 43.45507459029313679, 73.00433879953099847 ) ) ;
#4628 = CARTESIAN_POINT ( 'NONE',  ( 5.323881593982134675, 50.64173803113060757, 79.54845644658969661 ) ) ;
#4629 = EDGE_LOOP ( 'NONE', ( #5969, #10610, #14836, #9981, #17816, #14435 ) ) ;
#4630 = CARTESIAN_POINT ( 'NONE',  ( -4.233078557257877073, 37.50902643103172807, 77.20593245741272881 ) ) ;
#4631 = CARTESIAN_POINT ( 'NONE',  ( 8.242077797972765296, 41.41581020936537527, 77.48357784852399277 ) ) ;
#4632 = CARTESIAN_POINT ( 'NONE',  ( -3.467962453771612275, 40.50591351489412517, 94.75121379953098710 ) ) ;
#4633 = CIRCLE ( 'NONE', #6315, 8.199999999999995737 ) ;
#4634 = EDGE_CURVE ( 'NONE', #3932, #11013, #15061, .T. ) ;
#4635 = ORIENTED_EDGE ( 'NONE', *, *, #1901, .T. ) ;
#4636 = CARTESIAN_POINT ( 'NONE',  ( -7.774959294756113692, 41.22996117453095621, 78.61536821129558916 ) ) ;
#4637 = SURFACE_SIDE_STYLE ('',( #12744 ) ) ;
#4638 = DIRECTION ( 'NONE',  ( 1.000000000000000000, -1.110223024625156540E-16, 1.779391786395883043E-16 ) ) ;
#4639 = CARTESIAN_POINT ( 'NONE',  ( -5.784195910403845176, 44.99242805365518194, 95.88308880123798872 ) ) ;
#4640 =( NAMED_UNIT ( * ) SI_UNIT ( $, .STERADIAN. ) SOLID_ANGLE_UNIT ( ) );
#4641 = CARTESIAN_POINT ( 'NONE',  ( -5.782670150369643380, 50.47275727106970322, 76.07566230427023868 ) ) ;
#4642 = LINE ( 'NONE', #11583, #7899 ) ;
#4643 = DIRECTION ( 'NONE',  ( -1.540237394707283727E-16, -1.793354297423763257E-16, 1.000000000000000000 ) ) ;
#4644 = CARTESIAN_POINT ( 'NONE',  ( -0.7221989753287875180, 52.21573735104068703, 79.09854784679095019 ) ) ;
#4645 = CIRCLE ( 'NONE', #19259, 0.9921021478795020165 ) ;
#4646 = CARTESIAN_POINT ( 'NONE',  ( 1.855487073639841000, 49.49551470481302573, 69.82100546619766135 ) ) ;
#4647 = DIRECTION ( 'NONE',  ( 0.000000000000000000, 0.000000000000000000, 1.000000000000000000 ) ) ;
#4648 = CARTESIAN_POINT ( 'NONE',  ( 8.387651578222229176, 39.93204838481331365, 78.28891658965622469 ) ) ;
#4649 = CARTESIAN_POINT ( 'NONE',  ( 1.039473849130955418, 52.94750985498448870, 79.52524494518011977 ) ) ;
#4650 = VERTEX_POINT ( 'NONE', #575 ) ;
#4651 = EDGE_LOOP ( 'NONE', ( #16665, #20334, #7065, #9170 ) ) ;
#4652 = EDGE_CURVE ( 'NONE', #17731, #9962, #9972, .T. ) ;
#4653 = CARTESIAN_POINT ( 'NONE',  ( 8.244390605783030068, 41.39379493652497644, 75.36077184440998167 ) ) ;
#4654 = CARTESIAN_POINT ( 'NONE',  ( -3.798798875594516122, 36.41348040526440144, 79.26586447293075821 ) ) ;
#4655 = DIRECTION ( 'NONE',  ( -2.267473790562806355E-16, 5.922860397471811774E-17, -1.000000000000000000 ) ) ;
#4656 = CARTESIAN_POINT ( 'NONE',  ( -3.981178359372548492, 46.76218137147973408, 93.85183879953099506 ) ) ;
#4657 = CARTESIAN_POINT ( 'NONE',  ( 8.941883057029242465, 41.59311528658734147, 77.39218765127517941 ) ) ;
#4658 = AXIS2_PLACEMENT_3D ( 'NONE', #18051, #8269, #8159 ) ;
#4659 = CARTESIAN_POINT ( 'NONE',  ( 9.292527943876132568, 42.64402025696431764, 77.82525376769920911 ) ) ;
#4660 = CARTESIAN_POINT ( 'NONE',  ( 0.5221537403065118488, 48.16218137147969003, 45.55433879953100273 ) ) ;
#4661 = VERTEX_POINT ( 'NONE', #16865 ) ;
#4662 = CARTESIAN_POINT ( 'NONE',  ( -4.952297205838755545, 37.26552315606879517, 79.54733240137164785 ) ) ;
#4663 = EDGE_CURVE ( 'NONE', #2198, #16412, #16756, .T. ) ;
#4664 = DIRECTION ( 'NONE',  ( -1.402518428993831183E-16, 1.000000000000000000, 0.000000000000000000 ) ) ;
#4665 = ADVANCED_FACE ( 'NONE', ( #2283 ), #7928, .T. ) ;
#4666 = CARTESIAN_POINT ( 'NONE',  ( -3.379507664096216946, 36.94932017462306106, 77.62000880070094411 ) ) ;
#4667 = ORIENTED_EDGE ( 'NONE', *, *, #19903, .F. ) ;
#4668 = CARTESIAN_POINT ( 'NONE',  ( 0.5934291639749685876, 52.36187159818830850, 75.36022115247205022 ) ) ;
#4669 = EDGE_CURVE ( 'NONE', #19301, #2672, #20631, .T. ) ;
#4670 = EDGE_CURVE ( 'NONE', #5430, #5246, #17348, .T. ) ;
#4671 = CARTESIAN_POINT ( 'NONE',  ( 27.27315414062681853, 40.36218137147969287, 87.85433879953103542 ) ) ;
#4672 = ORIENTED_EDGE ( 'NONE', *, *, #21006, .T. ) ;
#4673 = CARTESIAN_POINT ( 'NONE',  ( 6.424237833264311526, 38.48359793996362299, 76.18799845131768222 ) ) ;
#4674 = CARTESIAN_POINT ( 'NONE',  ( 8.238767346824911186, 41.44068808925890579, 77.95380709400741637 ) ) ;
#4675 = CARTESIAN_POINT ( 'NONE',  ( 6.212565296439490403, 37.41256891269643603, 78.35997004935869370 ) ) ;
#4676 = PLANE ( 'NONE',  #4820 ) ;
#4677 = ORIENTED_EDGE ( 'NONE', *, *, #4678, .T. ) ;
#4678 = EDGE_CURVE ( 'NONE', #13937, #5501, #12593, .T. ) ;
#4679 = FACE_OUTER_BOUND ( 'NONE', #11386, .T. ) ;
#4680 = AXIS2_PLACEMENT_3D ( 'NONE', #8259, #13052, #13364 ) ;
#4681 = VERTEX_POINT ( 'NONE', #5961 ) ;
#4682 = CARTESIAN_POINT ( 'NONE',  ( -2.416137431568557314, 39.07291177436112406, 96.11746380123797451 ) ) ;
#4683 = DIRECTION ( 'NONE',  ( -1.540237394707284467E-16, -1.793354297423764243E-16, 1.000000000000000000 ) ) ;
#4684 = CARTESIAN_POINT ( 'NONE',  ( -7.425569853284181399, 47.94249712161214916, 78.80863703060173009 ) ) ;
#4685 = B_SPLINE_CURVE_WITH_KNOTS ( 'NONE', 3,
 ( #11089, #7988, #7775, #20634, #16079, #14254, #11189, #12988, #19252, #4666, #1285, #6064 ),
 .UNSPECIFIED., .F., .F.,
 ( 4, 2, 2, 2, 2, 4 ),
 ( 0.000000000000000000, 0.0003362723517171105499, 0.0006725447034342210998, 0.0008406808792927945081, 0.001008817055151368025, 0.001345089406868523949 ),
 .UNSPECIFIED. ) ;
#4686 = CARTESIAN_POINT ( 'NONE',  ( 4.178421596892070156, 40.17206517740157778, 94.75121379611698558 ) ) ;
#4687 = CARTESIAN_POINT ( 'NONE',  ( -5.955451856753747109, 38.00651308716548726, 76.73301527011911105 ) ) ;
#4688 = ORIENTED_EDGE ( 'NONE', *, *, #16483, .F. ) ;
#4689 = CARTESIAN_POINT ( 'NONE',  ( 8.240531579721347200, 41.39327284936243245, 76.03295302879951123 ) ) ;
#4690 = AXIS2_PLACEMENT_3D ( 'NONE', #2905, #786, #13761 ) ;
#4691 = ORIENTED_EDGE ( 'NONE', *, *, #15958, .F. ) ;
#4692 = CARTESIAN_POINT ( 'NONE',  ( -3.364492789658395377, 52.20069827791003547, 76.33204918460485544 ) ) ;
#4693 = EDGE_CURVE ( 'NONE', #3176, #14996, #9171, .T. ) ;
#4694 = CARTESIAN_POINT ( 'NONE',  ( -5.154188915835984375, 42.64120994080404614, 93.61746380123797451 ) ) ;
#4695 = CARTESIAN_POINT ( 'NONE',  ( -7.868132033238831369, 41.48904945220900942, 77.97272179757899835 ) ) ;
#4696 = ORIENTED_EDGE ( 'NONE', *, *, #5660, .F. ) ;
#4697 = CARTESIAN_POINT ( 'NONE',  ( 2.046082049342416109, 52.21940049450358856, 77.27552032814631389 ) ) ;
#4698 = CARTESIAN_POINT ( 'NONE',  ( 3.357643116058058208, 37.76218137147968434, 96.05433879953096721 ) ) ;
#4699 = CARTESIAN_POINT ( 'NONE',  ( -4.227598324046955014, 37.48485322674370224, 78.89954634079194307 ) ) ;
#4700 = CARTESIAN_POINT ( 'NONE',  ( -4.188116532274838377, 50.86525147400593738, 78.93463757479271692 ) ) ;
#4701 = LINE ( 'NONE', #9732, #11302 ) ;
#4702 = ORIENTED_EDGE ( 'NONE', *, *, #4061, .F. ) ;
#4703 = DIRECTION ( 'NONE',  ( 0.3165065846431827645, 0.9485903129789529098, 0.000000000000000000 ) ) ;
#4704 = CARTESIAN_POINT ( 'NONE',  ( 2.522153740306495529, 49.81903562097208749, 83.21119304902340730 ) ) ;
#4705 = ORIENTED_EDGE ( 'NONE', *, *, #8850, .T. ) ;
#4706 = CARTESIAN_POINT ( 'NONE',  ( 4.510527851286438406, 51.24252967697265149, 77.72408214165703555 ) ) ;
#4707 = CARTESIAN_POINT ( 'NONE',  ( 3.693419005614973383, 39.25792614782567114, 95.05433879953100984 ) ) ;
#4708 = CIRCLE ( 'NONE', #4365, 3.199999999999987743 ) ;
#4709 = CARTESIAN_POINT ( 'NONE',  ( 0.7411699536762380580, 52.95947911001109532, 78.88801344401531424 ) ) ;
#4710 = CARTESIAN_POINT ( 'NONE',  ( 0.7901638384306293172, 50.30062182352762079, 91.07933879782399345 ) ) ;
#4711 = CARTESIAN_POINT ( 'NONE',  ( 0.7901638384306286511, 50.30062182352762079, 92.17308879782397923 ) ) ;
#4712 = DIRECTION ( 'NONE',  ( -0.5941461771851693774, -0.8043570849667760481, -2.357623395011396791E-16 ) ) ;
#4713 = VECTOR ( 'NONE', #13908, 1000.000000000000000 ) ;
#4714 = CARTESIAN_POINT ( 'NONE',  ( -3.059272215776527304, 36.79205479859442818, 76.91456057462045237 ) ) ;
#4715 = ORIENTED_EDGE ( 'NONE', *, *, #11962, .T. ) ;
#4716 = CARTESIAN_POINT ( 'NONE',  ( 2.083608154845512317, 52.20176614783930802, 78.73916595950259989 ) ) ;
#4717 = AXIS2_PLACEMENT_3D ( 'NONE', #20304, #19212, #4138 ) ;
#4718 = ORIENTED_EDGE ( 'NONE', *, *, #18055, .T. ) ;
#4719 = CARTESIAN_POINT ( 'NONE',  ( 8.869748494521283888, 41.37692342661967615, 77.52492703482499792 ) ) ;
#4720 = CARTESIAN_POINT ( 'NONE',  ( 5.848951923618479931, 37.15274410921379911, 77.37492703482499223 ) ) ;
#4721 = CARTESIAN_POINT ( 'NONE',  ( 8.722153740306517022, 44.16218137147969003, 56.15433879953099705 ) ) ;
#4722 = CARTESIAN_POINT ( 'NONE',  ( -7.605668267552800010, 43.10965446021727132, 76.06610350541322418 ) ) ;
#4723 = ORIENTED_EDGE ( 'NONE', *, *, #7806, .F. ) ;
#4724 = AXIS2_PLACEMENT_3D ( 'NONE', #8702, #10202, #8380 ) ;
#4725 = CARTESIAN_POINT ( 'NONE',  ( -4.524181921268124462, 40.28999182795290324, 93.69558880123798872 ) ) ;
#4726 = ORIENTED_EDGE ( 'NONE', *, *, #15267, .T. ) ;
#4727 = CARTESIAN_POINT ( 'NONE',  ( -4.002011967609277576, 36.56358573041304538, 75.49480657079904233 ) ) ;
#4728 = DIRECTION ( 'NONE',  ( -0.5941461771851691553, -0.8043570849667760481, -2.357623395011396791E-16 ) ) ;
#4729 = CARTESIAN_POINT ( 'NONE',  ( 5.544968037009670780, 45.50804040601273925, 93.38308879953099506 ) ) ;
#4730 = ORIENTED_EDGE ( 'NONE', *, *, #1419, .F. ) ;
#4731 = CARTESIAN_POINT ( 'NONE',  ( -5.018595066975972685, 37.31449471545010965, 77.33253961758860839 ) ) ;
#4732 = CARTESIAN_POINT ( 'NONE',  ( 8.787982635420597433, 41.13186595976554116, 77.18134264024645574 ) ) ;
#4733 = CARTESIAN_POINT ( 'NONE',  ( 0.7901638384306293172, 50.30062182352762079, 90.92308879782397923 ) ) ;
#4734 = VECTOR ( 'NONE', #15789, 1000.000000000000000 ) ;
#4735 = ORIENTED_EDGE ( 'NONE', *, *, #4411, .F. ) ;
#4736 = LINE ( 'NONE', #11995, #217 ) ;
#4737 = DIRECTION ( 'NONE',  ( 0.000000000000000000, 0.000000000000000000, 1.000000000000000000 ) ) ;
#4738 = FACE_OUTER_BOUND ( 'NONE', #20127, .T. ) ;
#4739 = CARTESIAN_POINT ( 'NONE',  ( -4.567115856812060670, 47.10047254335474065, 90.96121380123797451 ) ) ;
#4740 = ADVANCED_FACE ( 'NONE', ( #18940 ), #17346, .F. ) ;
#4741 = CARTESIAN_POINT ( 'NONE',  ( -4.567115856812060670, 47.10047254335474065, 93.30496380123798872 ) ) ;
#4742 = CARTESIAN_POINT ( 'NONE',  ( -5.483735557913453462, 50.68636498614493036, 75.61447646545406087 ) ) ;
#4743 = DIRECTION ( 'NONE',  ( -1.402518428993831183E-16, 1.000000000000000000, -3.469446951953617640E-16 ) ) ;
#4744 = AXIS2_PLACEMENT_3D ( 'NONE', #18215, #29, #6608 ) ;
#4745 = CARTESIAN_POINT ( 'NONE',  ( 8.787982635420597433, 41.13186595976554116, 77.18134264024645574 ) ) ;
#4746 = DIRECTION ( 'NONE',  ( 0.01891643426601404346, 0.01351699135163154063, 0.9997296931968457923 ) ) ;
#4747 = CARTESIAN_POINT ( 'NONE',  ( -3.154801521863568325, 47.83913663364971569, 92.86286078555453116 ) ) ;
#4748 = AXIS2_PLACEMENT_3D ( 'NONE', #17464, #10887, #2887 ) ;
#4749 = ORIENTED_EDGE ( 'NONE', *, *, #15853, .F. ) ;
#4750 = FACE_OUTER_BOUND ( 'NONE', #4363, .T. ) ;
#4751 = CARTESIAN_POINT ( 'NONE',  ( 8.634055581509258559, 43.03495486475600984, 76.16967972087822147 ) ) ;
#4752 = CARTESIAN_POINT ( 'NONE',  ( 5.561486116954087677, 51.38024414653337146, 76.36928804473561172 ) ) ;
#4753 = CARTESIAN_POINT ( 'NONE',  ( 1.921644402852825451, 52.85035846467894771, 79.11952361228654240 ) ) ;
#4754 = ORIENTED_EDGE ( 'NONE', *, *, #2629, .F. ) ;
#4755 = AXIS2_PLACEMENT_3D ( 'NONE', #10190, #9878, #1886 ) ;
#4756 = VERTEX_POINT ( 'NONE', #6168 ) ;
#4757 = CARTESIAN_POINT ( 'NONE',  ( 0.8455950101471346736, 52.35579997042385259, 78.52566232894263010 ) ) ;
#4758 = PLANE ( 'NONE',  #11480 ) ;
#4759 = CARTESIAN_POINT ( 'NONE',  ( 6.778550821858020825, 50.48124747537763568, 77.88538524077617353 ) ) ;
#4760 = EDGE_CURVE ( 'NONE', #1769, #13579, #12984, .T. ) ;
#4761 = LINE ( 'NONE', #1491, #7601 ) ;
#4762 = B_SPLINE_SURFACE_WITH_KNOTS ( 'NONE', 3, 1, ( 
 ( #7725, #20988 ),
 ( #20887, #14313 ),
 ( #11036, #1233 ),
 ( #6223, #15821 ),
 ( #14206, #19200 ),
 ( #6422, #20682 ),
 ( #6318, #6117 ),
 ( #4615, #17506 ),
 ( #4716, #11137 ),
 ( #9544, #16027 ),
 ( #3148, #16131 ),
 ( #8036, #12931 ),
 ( #19410, #4829 ),
 ( #17817, #3247 ),
 ( #9747, #16230 ),
 ( #1654, #13138 ),
 ( #3345, #19516 ),
 ( #466, #19614 ),
 ( #14735, #11761 ),
 ( #4928, #359 ),
 ( #1963, #8566 ),
 ( #17921, #19823 ),
 ( #156, #8457 ) ),
 .UNSPECIFIED., .F., .F., .F.,
 ( 4, 1, 1, 1, 1, 1, 1, 1, 1, 1, 1, 1, 1, 1, 1, 1, 1, 1, 1, 1, 4 ),
 ( 2, 2 ),
 ( 0.000000000000000000, 0.04297438296114229617, 0.08348499068739016760, 0.1209138123397622833, 0.1552987673628354603, 0.1872381756066306413, 0.2161558137575471383, 0.2423469948807361607, 0.2659345218879605177, 0.3103547245860572290, 0.3557075913687650637, 0.4032107411089864146, 0.4537893912586022926, 0.5075094828293470473, 0.5641094501553882701, 0.6252262897377069972, 0.6910483815401738950, 0.7616865875262860408, 0.8363505414003653549, 0.9158720556281316760, 1.000000000000000000 ),
 ( 0.000000000000000000, 1.000000000000000000 ),
 .UNSPECIFIED. ) ;
#4763 = DIRECTION ( 'NONE',  ( 1.084202172485505420E-16, 1.000000000000000000, 0.000000000000000000 ) ) ;
#4764 = COLOUR_RGB ( '', 0.66274510, 0.83137255, 0.94901961) ;
#4765 = ADVANCED_FACE ( 'NONE', ( #3092 ), #11087, .T. ) ;
#4766 = CARTESIAN_POINT ( 'NONE',  ( 5.008975552073978932, 51.78836144432716537, 77.68963291717794561 ) ) ;
#4767 = CARTESIAN_POINT ( 'NONE',  ( 6.569564547327074955, 50.63561721789299952, 77.67636243622263237 ) ) ;
#4768 = CARTESIAN_POINT ( 'NONE',  ( -3.053082554203017995, 36.78748274492484427, 76.62933879953087057 ) ) ;
#4769 = CARTESIAN_POINT ( 'NONE',  ( -7.677846259693478892, 49.36218137147968577, 93.55433879953098142 ) ) ;
#4770 = EDGE_LOOP ( 'NONE', ( #19229, #942 ) ) ;
#4771 = CYLINDRICAL_SURFACE ( 'NONE', #6473, 5.199999999999999289 ) ;
#4772 = EDGE_CURVE ( 'NONE', #9577, #15919, #9592, .T. ) ;
#4773 = DIRECTION ( 'NONE',  ( -1.779391786395883783E-16, -5.922860397471806844E-17, 1.000000000000000000 ) ) ;
#4774 = CARTESIAN_POINT ( 'NONE',  ( 0.5221537403065042993, 44.16218137147969713, 85.55433879953100984 ) ) ;
#4775 = EDGE_CURVE ( 'NONE', #618, #3158, #7878, .T. ) ;
#4776 = LINE ( 'NONE', #11301, #2403 ) ;
#4777 = CARTESIAN_POINT ( 'NONE',  ( 8.707758170209565662, 40.89142814818289651, 75.40210940951681096 ) ) ;
#4778 = ORIENTED_EDGE ( 'NONE', *, *, #11818, .F. ) ;
#4779 = CARTESIAN_POINT ( 'NONE',  ( -0.4031263708652977340, 52.21524339649662494, 75.56421855115301867 ) ) ;
#4780 = CARTESIAN_POINT ( 'NONE',  ( -1.590937568396970203, 39.63064243629642647, 94.51683879611698558 ) ) ;
#4781 = CARTESIAN_POINT ( 'NONE',  ( 6.228842675835584153, 38.34397571433836305, 78.14418354478426920 ) ) ;
#4782 = CARTESIAN_POINT ( 'NONE',  ( 0.7627568828200497197, 52.96425867272768784, 76.01945459498423929 ) ) ;
#4783 = CARTESIAN_POINT ( 'NONE',  ( 5.434012744193106315, 45.09686908721048582, 92.45433879953098710 ) ) ;
#4784 = EDGE_CURVE ( 'NONE', #2902, #7082, #9799, .T. ) ;
#4785 = ORIENTED_EDGE ( 'NONE', *, *, #19357, .F. ) ;
#4786 = VECTOR ( 'NONE', #10015, 1000.000000000000000 ) ;
#4787 = EDGE_CURVE ( 'NONE', #6827, #16377, #8677, .T. ) ;
#4788 = CARTESIAN_POINT ( 'NONE',  ( 8.930560609631596591, 41.55918119345393080, 76.05553801048951357 ) ) ;
#4789 = EDGE_CURVE ( 'NONE', #2032, #2305, #19381, .T. ) ;
#4790 = ORIENTED_EDGE ( 'NONE', *, *, #11754, .F. ) ;
#4791 = CARTESIAN_POINT ( 'NONE',  ( -5.154188915835984375, 42.64120994080404614, 94.71121380123797451 ) ) ;
#4792 = CARTESIAN_POINT ( 'NONE',  ( 4.394343283833276992, 39.11584570990505938, 92.60183880123797451 ) ) ;
#4793 = CYLINDRICAL_SURFACE ( 'NONE', #21007, 4.200000000000001066 ) ;
#4794 = CARTESIAN_POINT ( 'NONE',  ( 25.03948732994508219, 45.16218137147969003, 74.70433879953100131 ) ) ;
#4795 = DIRECTION ( 'NONE',  ( -0.5941461771851691553, -0.8043570849667760481, -2.357623395011396791E-16 ) ) ;
#4796 = ADVANCED_FACE ( 'NONE', ( #19355 ), #4771, .F. ) ;
#4797 = VECTOR ( 'NONE', #1452, 1000.000000000000114 ) ;
#4798 = ORIENTED_EDGE ( 'NONE', *, *, #12448, .T. ) ;
#4799 = DIRECTION ( 'NONE',  ( -1.000000000000000000, 1.110223024625156540E-16, -1.779391786395883043E-16 ) ) ;
#4800 = AXIS2_PLACEMENT_3D ( 'NONE', #6517, #19187, #8019 ) ;
#4801 =( BOUNDED_CURVE ( )  B_SPLINE_CURVE ( 3, ( #3120, #9623, #1527, #8943 ),
 .UNSPECIFIED., .F., .F. ) 
 B_SPLINE_CURVE_WITH_KNOTS ( ( 4, 4 ),
 ( 5.988669822071447157, 6.577700792287721754 ),
 .UNSPECIFIED. ) 
 CURVE ( )  GEOMETRIC_REPRESENTATION_ITEM ( )  RATIONAL_B_SPLINE_CURVE ( ( 1.000000000000000000, 0.9712952651971044071, 0.9712952651971044071, 1.000000000000000000 ) ) 
 REPRESENTATION_ITEM ( '' )  );
#4802 = ORIENTED_EDGE ( 'NONE', *, *, #18489, .T. ) ;
#4803 = CARTESIAN_POINT ( 'NONE',  ( 26.43948732994507367, 36.35905713404684292, 74.70433879953098710 ) ) ;
#4804 = PLANE ( 'NONE',  #6841 ) ;
#4805 = CARTESIAN_POINT ( 'NONE',  ( -5.784195910403845176, 44.99242805365518194, 94.63308880123798872 ) ) ;
#4806 = ORIENTED_EDGE ( 'NONE', *, *, #16023, .T. ) ;
#4807 = LINE ( 'NONE', #11327, #19796 ) ;
#4808 = CARTESIAN_POINT ( 'NONE',  ( -5.428519676309859321, 37.61728951159455647, 79.46937556254052026 ) ) ;
#4809 = CARTESIAN_POINT ( 'NONE',  ( -4.705149740856864327, 37.08296527939383225, 78.93669174070734584 ) ) ;
#4810 = CARTESIAN_POINT ( 'NONE',  ( 5.239803326269729666, 50.86322232383581365, 76.04240903267428564 ) ) ;
#4811 = DIRECTION ( 'NONE',  ( 5.213532094855085691E-33, -3.469446951953617640E-16, -1.000000000000000000 ) ) ;
#4812 = VERTEX_POINT ( 'NONE', #18395 ) ;
#4813 = CARTESIAN_POINT ( 'NONE',  ( -4.133436435564208367, 50.90432386914923768, 75.98707017319573254 ) ) ;
#4814 = CARTESIAN_POINT ( 'NONE',  ( 8.912633302440582383, 46.81545344901155659, 80.45433879953087342 ) ) ;
#4815 = VECTOR ( 'NONE', #14128, 1000.000000000000114 ) ;
#4816 = ORIENTED_EDGE ( 'NONE', *, *, #364, .F. ) ;
#4817 = CARTESIAN_POINT ( 'NONE',  ( 4.582010541884842247, 52.10374329815417127, 78.30859729819620441 ) ) ;
#4818 = EDGE_CURVE ( 'NONE', #2000, #9137, #11808, .T. ) ;
#4819 = DIRECTION ( 'NONE',  ( 0.3165065846431827645, 0.9485903129789529098, 0.000000000000000000 ) ) ;
#4820 = AXIS2_PLACEMENT_3D ( 'NONE', #7892, #17671, #1297 ) ;
#4821 = CARTESIAN_POINT ( 'NONE',  ( -5.706182906969134550, 50.52741225482698439, 75.88700421999355683 ) ) ;
#4822 = CARTESIAN_POINT ( 'NONE',  ( 5.053692675489762642, 42.04909006277621586, 93.57933879611698558 ) ) ;
#4823 = CARTESIAN_POINT ( 'NONE',  ( 5.856396280011940014, 46.10368687828906076, 93.18871379782397923 ) ) ;
#4824 = EDGE_CURVE ( 'NONE', #16863, #5156, #8135, .T. ) ;
#4825 = CARTESIAN_POINT ( 'NONE',  ( -1.677846259693499542, 44.16218137147969003, 50.15433879953098995 ) ) ;
#4826 = EDGE_CURVE ( 'NONE', #15617, #9093, #2225, .T. ) ;
#4827 = CARTESIAN_POINT ( 'NONE',  ( -3.639202304192273640, 36.29559284691160315, 77.48323649892105891 ) ) ;
#4828 = VERTEX_POINT ( 'NONE', #3604 ) ;
#4829 = CARTESIAN_POINT ( 'NONE',  ( 1.940234681537338801, 52.95557165619788265, 79.09265199143256098 ) ) ;
#4830 = DIRECTION ( 'NONE',  ( -0.9534635866061451637, -0.3015081906286224411, -2.009271279954815058E-16 ) ) ;
#4831 = ORIENTED_EDGE ( 'NONE', *, *, #2173, .F. ) ;
#4832 = VECTOR ( 'NONE', #11745, 1000.000000000000227 ) ;
#4833 = CARTESIAN_POINT ( 'NONE',  ( -7.780652970462169193, 41.24611481839983895, 78.48594744126245359 ) ) ;
#4834 = VECTOR ( 'NONE', #1170, 1000.000000000000227 ) ;
#4835 = CARTESIAN_POINT ( 'NONE',  ( -4.477846259693498254, 36.96218137147968008, 53.35433879953099989 ) ) ;
#4836 = CARTESIAN_POINT ( 'NONE',  ( -7.590232248627324374, 43.06084092073458436, 76.13058770837619704 ) ) ;
#4837 = VERTEX_POINT ( 'NONE', #10334 ) ;
#4838 = CARTESIAN_POINT ( 'NONE',  ( 2.891178777429407099, 49.58011692473793630, 94.41981103945796860 ) ) ;
#4839 = CARTESIAN_POINT ( 'NONE',  ( -4.269064254816391291, 37.69685299354377861, 75.36022115247205022 ) ) ;
#4840 = ORIENTED_EDGE ( 'NONE', *, *, #5484, .T. ) ;
#4841 = CARTESIAN_POINT ( 'NONE',  ( 5.008975552073978932, 51.78836144432716537, 77.68963291717794561 ) ) ;
#4842 = LINE ( 'NONE', #6132, #13573 ) ;
#4843 = CARTESIAN_POINT ( 'NONE',  ( -0.2125050281363792815, 38.58189400963055959, 95.49246379953098085 ) ) ;
#4844 = VERTEX_POINT ( 'NONE', #12029 ) ;
#4845 = CARTESIAN_POINT ( 'NONE',  ( 0.5221537403065015237, 44.16218137147968292, 75.45433879953087342 ) ) ;
#4846 = CARTESIAN_POINT ( 'NONE',  ( -4.759934653634315893, 37.89819380636689061, 77.90166954077812989 ) ) ;
#4847 = CARTESIAN_POINT ( 'NONE',  ( 5.928963754087452465, 43.92611494815086814, 92.71996379953098710 ) ) ;
#4848 = VERTEX_POINT ( 'NONE', #5194 ) ;
#4849 = PLANE ( 'NONE',  #10096 ) ;
#4850 = DIRECTION ( 'NONE',  ( 1.540237394707283727E-16, 1.793354297423763257E-16, -1.000000000000000000 ) ) ;
#4851 = LINE ( 'NONE', #11157, #4 ) ;
#4852 = AXIS2_PLACEMENT_3D ( 'NONE', #4814, #5417, #11337 ) ;
#4853 = UNCERTAINTY_MEASURE_WITH_UNIT (LENGTH_MEASURE( 1.000000000000000082E-05 ), #4544, 'distance_accuracy_value', 'NONE');
#4854 = CARTESIAN_POINT ( 'NONE',  ( 29.03948732994507864, 43.16218137147969003, 74.70433879953100131 ) ) ;
#4855 = CARTESIAN_POINT ( 'NONE',  ( -1.440187084481231894, 38.28092143101017797, 78.25433879953088478 ) ) ;
#4856 = FACE_OUTER_BOUND ( 'NONE', #17476, .T. ) ;
#4857 = AXIS2_PLACEMENT_3D ( 'NONE', #6529, #20983, #11346 ) ;
#4858 = VERTEX_POINT ( 'NONE', #3702 ) ;
#4859 = LINE ( 'NONE', #17957, #17648 ) ;
#4860 = CARTESIAN_POINT ( 'NONE',  ( 11.22215374030649926, 42.96218137147968008, 77.40433879953098995 ) ) ;
#4861 = CARTESIAN_POINT ( 'NONE',  ( 8.535530527220215546, 40.37525097622586401, 79.30521328845429707 ) ) ;
#4862 = CARTESIAN_POINT ( 'NONE',  ( 6.138829900063904610, 50.03976854554820619, 77.70577767651062118 ) ) ;
#4863 = ORIENTED_EDGE ( 'NONE', *, *, #16806, .F. ) ;
#4864 = AXIS2_PLACEMENT_3D ( 'NONE', #9476, #19049, #11081 ) ;
#4865 = ADVANCED_FACE ( 'NONE', ( #10112 ), #4244, .F. ) ;
#4866 = DIRECTION ( 'NONE',  ( -1.540237394707284467E-16, -1.793354297423764243E-16, 1.000000000000000000 ) ) ;
#4867 = DIRECTION ( 'NONE',  ( -1.571217453038212812E-16, -0.7071067811865500152, -0.7071067811865451302 ) ) ;
#4868 = DIRECTION ( 'NONE',  ( -1.540237394707284220E-16, -1.793354297423764243E-16, 1.000000000000000000 ) ) ;
#4869 = CARTESIAN_POINT ( 'NONE',  ( 5.666884522201894647, 41.76315400873614436, 94.28246379782397923 ) ) ;
#4870 = DIRECTION ( 'NONE',  ( -0.5813877811927011807, 0.8136266022444372803, 5.636455622144619183E-17 ) ) ;
#4871 = CARTESIAN_POINT ( 'NONE',  ( 0.3293525775907221176, 52.35991604324109971, 77.67332569164774725 ) ) ;
#4872 = CARTESIAN_POINT ( 'NONE',  ( 6.446086404075624721, 49.80199260132323502, 77.33077842133744184 ) ) ;
#4873 = DIRECTION ( 'NONE',  ( -0.5813877811927011807, 0.8136266022444372803, 5.636455622144619183E-17 ) ) ;
#4874 = AXIS2_PLACEMENT_3D ( 'NONE', #11351, #15822, #13043 ) ;
#4875 = CARTESIAN_POINT ( 'NONE',  ( 4.394343283833276992, 39.11584570990505938, 91.35183880123798872 ) ) ;
#4876 = VERTEX_POINT ( 'NONE', #14783 ) ;
#4877 = CARTESIAN_POINT ( 'NONE',  ( -5.769203958596529347, 48.43638519259696551, 72.45432679953087529 ) ) ;
#4878 = VERTEX_POINT ( 'NONE', #19667 ) ;
#4879 = CARTESIAN_POINT ( 'NONE',  ( -5.832343694407396306, 50.43726237516484900, 78.41225960292398156 ) ) ;
#4880 = EDGE_CURVE ( 'NONE', #1872, #7531, #203, .T. ) ;
#4881 = CARTESIAN_POINT ( 'NONE',  ( 6.012275498921958672, 37.26944915646792822, 78.37198585835440667 ) ) ;
#4882 = MANIFOLD_SOLID_BREP ( 'Stock-MAS-160-1', #5077 ) ;
#4883 = CARTESIAN_POINT ( 'NONE',  ( 8.889236131602293867, 41.43532911122410667, 77.52218233473911368 ) ) ;
#4884 = CARTESIAN_POINT ( 'NONE',  ( 9.035997676120972599, 41.87518277052537030, 78.13634973986094678 ) ) ;
#4885 = ORIENTED_EDGE ( 'NONE', *, *, #7288, .T. ) ;
#4886 = CARTESIAN_POINT ( 'NONE',  ( 0.1862881254137638554, 52.21059564658006025, 75.38460717221940399 ) ) ;
#4887 = CARTESIAN_POINT ( 'NONE',  ( 0.2893871155212132673, 52.97020135390489060, 79.53425070713537082 ) ) ;
#4888 = CARTESIAN_POINT ( 'NONE',  ( 0.5221537403065005245, 44.16218137147968292, 82.45433879953087342 ) ) ;
#4889 = CARTESIAN_POINT ( 'NONE',  ( 4.108651072766817514, 51.53644210273448323, 76.21360399200699476 ) ) ;
#4890 = CARTESIAN_POINT ( 'NONE',  ( 0.5221537403065019678, 44.16218137147968292, 72.45433879953087342 ) ) ;
#4891 = ORIENTED_EDGE ( 'NONE', *, *, #11997, .F. ) ;
#4892 = CARTESIAN_POINT ( 'NONE',  ( 1.771153339986189845, 40.36218137147969998, 46.35433879953098568 ) ) ;
#4893 = ADVANCED_FACE ( 'NONE', ( #5723 ), #15320, .T. ) ;
#4894 = ORIENTED_EDGE ( 'NONE', *, *, #14802, .F. ) ;
#4895 = CARTESIAN_POINT ( 'NONE',  ( -5.154188915835984375, 42.64120994080404614, 92.21121380123797451 ) ) ;
#4896 = CARTESIAN_POINT ( 'NONE',  ( -7.813542802050427838, 46.98339118501086631, 79.23467789972187347 ) ) ;
#4897 = DIRECTION ( 'NONE',  ( 1.402518428993831676E-16, -1.000000000000000000, 0.000000000000000000 ) ) ;
#4898 = CARTESIAN_POINT ( 'NONE',  ( -7.324551137483023666, 41.80748339028045280, 78.91811502121268518 ) ) ;
#4899 = ADVANCED_FACE ( 'NONE', ( #732 ), #1557, .T. ) ;
#4900 = DIRECTION ( 'NONE',  ( 1.000000000000000000, 0.000000000000000000, 0.000000000000000000 ) ) ;
#4901 = VERTEX_POINT ( 'NONE', #5837 ) ;
#4902 = CARTESIAN_POINT ( 'NONE',  ( -4.557243880370988265, 36.97371317826440418, 76.05537227506185616 ) ) ;
#4903 = EDGE_LOOP ( 'NONE', ( #41, #1774, #515, #2025 ) ) ;
#4904 = CARTESIAN_POINT ( 'NONE',  ( -7.649386493801853426, 47.42852896470760982, 78.28566691767271379 ) ) ;
#4905 = CARTESIAN_POINT ( 'NONE',  ( 5.753005855668248181, 51.23877623043087937, 78.93669174070734584 ) ) ;
#4906 = CARTESIAN_POINT ( 'NONE',  ( 1.352400422481993658, 50.46853102219002096, 94.32058880123798872 ) ) ;
#4907 = ORIENTED_EDGE ( 'NONE', *, *, #19710, .F. ) ;
#4908 = CARTESIAN_POINT ( 'NONE',  ( -5.838300394258943093, 50.43300593553962585, 78.21416447440572028 ) ) ;
#4909 = CARTESIAN_POINT ( 'NONE',  ( -4.952297205838751992, 37.26552315606879517, 79.54733240137164785 ) ) ;
#4911 = CARTESIAN_POINT ( 'NONE',  ( 5.928804517645879457, 51.10892084043006633, 76.16996516156804375 ) ) ;
#4910 = B_SPLINE_CURVE_WITH_KNOTS ( 'NONE', 3,
 ( #10445, #14036, #5946, #18924, #12132, #4648, #2763, #6254, #9468, #15751, #14559, #17752, #3074, #10968, #7969, #19333, #9266, #4861, #15953, #17637, #1263, #15849, #7654, #20826, #2863, #20716, #16163 ),
 .UNSPECIFIED., .F., .F.,
 ( 4, 1, 1, 1, 1, 1, 1, 1, 1, 1, 1, 1, 1, 1, 1, 1, 1, 1, 1, 1, 1, 1, 1, 1, 4 ),
 ( 0.000000000000000000, 0.05993306358482522467, 0.1145105083304139432, 0.1639926324650750333, 0.2083799252409545000, 0.2474206522578790979, 0.2813744068707942358, 0.3102651545178817805, 0.3340707221093189849, 0.3764843156245091249, 0.4195869878574357559, 0.4649490021377667981, 0.5131068515344550107, 0.5381792345077858197, 0.5638273912065150384, 0.5896398555221948889, 0.6163062535856453916, 0.6433841197412238921, 0.6712141767968796691, 0.7000136030487154049, 0.7297781433983795418, 0.7919609919944711196, 0.8575419152218471952, 0.9267698348267595643, 1.000000000000000000 ),
 .UNSPECIFIED. ) ;
#4912 = CARTESIAN_POINT ( 'NONE',  ( -4.030277663924256792, 50.97803735047946105, 78.47566305278908771 ) ) ;
#4913 = CARTESIAN_POINT ( 'NONE',  ( 3.873544841512767789, 48.16470079461350906, 93.50578198602111968 ) ) ;
#4914 = ORIENTED_EDGE ( 'NONE', *, *, #7439, .F. ) ;
#4915 = LINE ( 'NONE', #19813, #6441 ) ;
#4916 = DIRECTION ( 'NONE',  ( 0.000000000000000000, 0.000000000000000000, -1.000000000000000000 ) ) ;
#4917 = VERTEX_POINT ( 'NONE', #12343 ) ;
#4918 = CARTESIAN_POINT ( 'NONE',  ( -2.294692865963147810, 48.87505292694043391, 95.05433879953096721 ) ) ;
#4919 = CARTESIAN_POINT ( 'NONE',  ( -7.419120997399995865, 40.07157761357974124, 78.50801527011910252 ) ) ;
#4920 = CARTESIAN_POINT ( 'NONE',  ( -4.699374957658429608, 51.24684035381270064, 75.36124333316173818 ) ) ;
#4921 = CARTESIAN_POINT ( 'NONE',  ( -3.467962453771613607, 40.50591351489412517, 95.68871379611699979 ) ) ;
#4922 = LINE ( 'NONE', #12815, #7252 ) ;
#4923 =( BOUNDED_CURVE ( )  B_SPLINE_CURVE ( 2, ( #9943, #449, #10044, #6931, #5331, #11843, #16428 ),
 .UNSPECIFIED., .F., .T. ) 
 B_SPLINE_CURVE_WITH_KNOTS ( ( 3, 2, 2, 3 ),
 ( 0.2122652878748581273, 0.2187500000000000000, 0.2500000000000000000, 0.2673390146554854296 ),
 .UNSPECIFIED. ) 
 CURVE ( )  GEOMETRIC_REPRESENTATION_ITEM ( )  RATIONAL_B_SPLINE_CURVE ( ( 0.9749639689766236295, 0.9842041818081431748, 1.000000000000000000, 0.9238795325112867385, 1.000000000000000000, 0.9577646751561855742, 0.9623977609649205789 ) ) 
 REPRESENTATION_ITEM ( '' )  );
#4924 = DIRECTION ( 'NONE',  ( -0.5941461771851691553, -0.8043570849667760481, -2.357623395011396791E-16 ) ) ;
#4925 = CARTESIAN_POINT ( 'NONE',  ( 5.619997200715287633, 36.98914144679460492, 77.75986257808632729 ) ) ;
#4926 = CARTESIAN_POINT ( 'NONE',  ( 5.504825744318520897, 50.66746093937735651, 76.01152026380901816 ) ) ;
#4927 = VERTEX_POINT ( 'NONE', #1683 ) ;
#4928 = CARTESIAN_POINT ( 'NONE',  ( 1.023998609437386520, 52.21012155851776981, 79.52671882365912381 ) ) ;
#4929 = DIRECTION ( 'NONE',  ( -0.3165065846431775465, -0.9485903129789546862, 0.000000000000000000 ) ) ;
#4930 = EDGE_CURVE ( 'NONE', #13218, #2822, #20914, .T. ) ;
#4931 = ORIENTED_EDGE ( 'NONE', *, *, #13920, .T. ) ;
#4932 = CARTESIAN_POINT ( 'NONE',  ( -7.831411425717313968, 41.39424600171143709, 78.12842291999400857 ) ) ;
#4933 = EDGE_CURVE ( 'NONE', #19814, #14654, #5399, .T. ) ;
#4934 = DIRECTION ( 'NONE',  ( -1.402518428993831676E-16, 1.000000000000000000, 0.000000000000000000 ) ) ;
#4935 = CARTESIAN_POINT ( 'NONE',  ( 9.060635047751631532, 41.94902253626816702, 79.49775514261133935 ) ) ;
#4936 = B_SPLINE_SURFACE_WITH_KNOTS ( 'NONE', 3, 1, ( 
 ( #20579, #6005 ),
 ( #2921, #4201 ),
 ( #17288, #14096 ),
 ( #12503, #12305 ),
 ( #15811, #1224 ),
 ( #10726, #13882 ),
 ( #7393, #17187 ),
 ( #15597, #5912 ),
 ( #7713, #12610 ),
 ( #20365, #18787 ),
 ( #20671, #19096 ),
 ( #16436, #2142 ),
 ( #9837, #6622 ),
 ( #3439, #17808 ),
 ( #3022, #13126 ) ),
 .UNSPECIFIED., .F., .F., .F.,
 ( 4, 1, 1, 1, 1, 1, 1, 1, 1, 1, 1, 1, 4 ),
 ( 2, 2 ),
 ( 0.000000000000000000, 0.07572900668544887970, 0.1557212283653267859, 0.2428008865684916084, 0.3367971223029513350, 0.3882775785060046392, 0.4462854066205887982, 0.5120087213739217269, 0.5869354790617866691, 0.6733690469438747828, 0.7707158190319922664, 0.8795326993170452523, 1.000000000000000000 ),
 ( 0.000000000000000000, 1.000000000000000000 ),
 .UNSPECIFIED. ) ;
#4937 = EDGE_LOOP ( 'NONE', ( #11043, #3843, #17393, #11659 ) ) ;
#4938 = CARTESIAN_POINT ( 'NONE',  ( -3.416655834010613013, 49.09312775492363556, 93.38736517557353523 ) ) ;
#4939 = CARTESIAN_POINT ( 'NONE',  ( -5.362906160289790947, 38.50482994647732227, 75.80435357840198662 ) ) ;
#4940 = ORIENTED_EDGE ( 'NONE', *, *, #15640, .F. ) ;
#4941 = CARTESIAN_POINT ( 'NONE',  ( 0.5221537403065081850, 50.16218137147969713, 67.55433879953099563 ) ) ;
#4942 = CARTESIAN_POINT ( 'NONE',  ( 0.3326973149608336566, 52.96014171822455552, 77.10139762306027933 ) ) ;
#4943 = ADVANCED_FACE ( 'NONE', ( #4548 ), #9570, .F. ) ;
#4944 = CARTESIAN_POINT ( 'NONE',  ( 3.122153740306552905, 48.66551347115873227, 94.78933879953099506 ) ) ;
#4945 = ORIENTED_EDGE ( 'NONE', *, *, #9687, .T. ) ;
#4946 = CARTESIAN_POINT ( 'NONE',  ( -4.765255033702754162, 37.90212375680545875, 77.33633635728615729 ) ) ;
#4947 = CARTESIAN_POINT ( 'NONE',  ( -3.154801521863568325, 47.83913663364971569, 83.28180655319408743 ) ) ;
#4948 = CARTESIAN_POINT ( 'NONE',  ( 5.220616844236030119, 45.87228208810806507, 94.04808879953097289 ) ) ;
#4949 = ADVANCED_FACE ( 'NONE', ( #4856 ), #19327, .T. ) ;
#4950 = ORIENTED_EDGE ( 'NONE', *, *, #2854, .F. ) ;
#4951 = CARTESIAN_POINT ( 'NONE',  ( -4.795362370604993707, 51.17825126284458293, 76.19771883405211099 ) ) ;
#4952 = FACE_OUTER_BOUND ( 'NONE', #8523, .T. ) ;
#4953 = CARTESIAN_POINT ( 'NONE',  ( 2.119851040271390374, 52.81592988514039178, 76.48963291717792856 ) ) ;
#4954 = CARTESIAN_POINT ( 'NONE',  ( 5.611423337425062385, 41.22389019960463230, 93.92996380123798872 ) ) ;
#4955 = DIRECTION ( 'NONE',  ( 1.000000000000000000, 0.000000000000000000, 0.000000000000000000 ) ) ;
#4956 = CARTESIAN_POINT ( 'NONE',  ( -4.435834490810350417, 37.63071868037679479, 75.97716382624557241 ) ) ;
#4957 = CYLINDRICAL_SURFACE ( 'NONE', #408, 8.199999999999995737 ) ;
#4958 = CARTESIAN_POINT ( 'NONE',  ( 3.961507247562192635, 36.71833509068318335, 76.73963291717792856 ) ) ;
#4959 = CARTESIAN_POINT ( 'NONE',  ( 7.684216168072399711, 40.18822588599692125, 78.67376765716130649 ) ) ;
#4960 = ORIENTED_EDGE ( 'NONE', *, *, #1259, .T. ) ;
#4961 = DIRECTION ( 'NONE',  ( -0.5941461771851691553, -0.8043570849667760481, -2.357623395011396791E-16 ) ) ;
#4962 = CARTESIAN_POINT ( 'NONE',  ( 9.353600933836910158, 42.82705988227500882, 76.64232882509132594 ) ) ;
#4963 = CARTESIAN_POINT ( 'NONE',  ( 11.22215374030650281, 42.96218137147968008, 61.40715055817103263 ) ) ;
#4964 = CARTESIAN_POINT ( 'NONE',  ( 2.063676922390465851, 52.82613311267615330, 78.85822911341185204 ) ) ;
#4965 = ORIENTED_EDGE ( 'NONE', *, *, #12611, .T. ) ;
#4966 = AXIS2_PLACEMENT_3D ( 'NONE', #18702, #17527, #5935 ) ;
#4967 = EDGE_CURVE ( 'NONE', #15461, #2251, #3177, .T. ) ;
#4968 = DIRECTION ( 'NONE',  ( -1.540237394707284220E-16, -1.793354297423764243E-16, 1.000000000000000000 ) ) ;
#4969 = ORIENTED_EDGE ( 'NONE', *, *, #7164, .T. ) ;
#4970 = B_SPLINE_CURVE_WITH_KNOTS ( 'NONE', 3,
 ( #19146, #7868, #1269, #6258, #18930, #20525, #5852, #18832, #13939, #17231 ),
 .UNSPECIFIED., .F., .F.,
 ( 4, 2, 2, 2, 4 ),
 ( 0.000000000000000000, 0.0002697494009883096770, 0.0003371867512354173591, 0.0004046241014825250411, 0.0005394988019767708171 ),
 .UNSPECIFIED. ) ;
#4971 = CARTESIAN_POINT ( 'NONE',  ( -2.083470957239372368, 47.45622447009557021, 79.40903933791013003 ) ) ;
#4972 = DIRECTION ( 'NONE',  ( -0.9999689119394085113, 0.007885122365275776257, -1.526048693634352652E-16 ) ) ;
#4973 = CARTESIAN_POINT ( 'NONE',  ( 8.787829143201872029, 41.13140593384864729, 78.45948585835439815 ) ) ;
#4974 = CARTESIAN_POINT ( 'NONE',  ( -5.462576778579502523, 43.73439565840071452, 82.45433879953087342 ) ) ;
#4975 = FACE_OUTER_BOUND ( 'NONE', #1424, .T. ) ;
#4976 = B_SPLINE_CURVE_WITH_KNOTS ( 'NONE', 3,
 ( #17461, #9284, #1501, #14149, #4467, #2884, #9382, #14252, #20736, #12675, #19156, #8516, #14784, #20939, #1, #2018, #14680, #6372, #1605, #3606, #6799, #11506, #4879, #5196, #17977, #6480, #19564 ),
 .UNSPECIFIED., .F., .F.,
 ( 4, 1, 1, 1, 1, 1, 1, 1, 1, 1, 1, 1, 1, 1, 1, 1, 1, 1, 1, 1, 1, 1, 1, 1, 4 ),
 ( 0.000000000000000000, 0.08415130211954198469, 0.1639620550106605512, 0.2403084560778752377, 0.3136616503690570767, 0.3487238096526073527, 0.3821668720153286181, 0.4136737894986983743, 0.4437099131648768457, 0.4722505124987256275, 0.4989577201472497614, 0.5245780966751731889, 0.5489676856186370690, 0.5954867311152326481, 0.6405007172309487018, 0.6844907576478919120, 0.7283883565803446203, 0.7516682776372889396, 0.7779555554382332483, 0.8073737814008299374, 0.8396655338036946858, 0.8751296329422569853, 0.9135058715745314473, 0.9551265033309996877, 1.000000000000000000 ),
 .UNSPECIFIED. ) ;
#4977 = CARTESIAN_POINT ( 'NONE',  ( -1.219056181836355446, 49.77488197367695477, 93.15612966814926210 ) ) ;
#4978 = CARTESIAN_POINT ( 'NONE',  ( 6.931410089129659724, 50.36833649219094866, 77.12327887040382279 ) ) ;
#4979 = CARTESIAN_POINT ( 'NONE',  ( -3.496029822981027380, 36.18983710238020279, 76.51650556680409920 ) ) ;
#4980 = LINE ( 'NONE', #7400, #6918 ) ;
#4981 = AXIS2_PLACEMENT_3D ( 'NONE', #13972, #2687, #7591 ) ;
#4982 = CARTESIAN_POINT ( 'NONE',  ( 6.828503391016846891, 43.33193468930419101, 91.50808880123798872 ) ) ;
#4983 = ORIENTED_EDGE ( 'NONE', *, *, #17178, .F. ) ;
#4984 = DIRECTION ( 'NONE',  ( 1.000000000000000000, 1.402518428993831676E-16, 0.000000000000000000 ) ) ;
#4985 = CARTESIAN_POINT ( 'NONE',  ( 8.865792162213244509, 41.36506604770743678, 78.93669174070734584 ) ) ;
#4986 = CARTESIAN_POINT ( 'NONE',  ( -4.853223633226585676, 37.19234149890714036, 78.86751516113972116 ) ) ;
#4987 = CARTESIAN_POINT ( 'NONE',  ( 2.263811127080450625, 49.90383875825364157, 85.41268141275705261 ) ) ;
#4988 = CARTESIAN_POINT ( 'NONE',  ( 9.222679282817953350, 42.43467938865651945, 77.98843304575544266 ) ) ;
#4989 = EDGE_LOOP ( 'NONE', ( #5014, #13382, #18582, #5579 ) ) ;
#4990 = VERTEX_POINT ( 'NONE', #14346 ) ;
#4991 = CARTESIAN_POINT ( 'NONE',  ( 6.882613847952937292, 37.89136107556471700, 76.65924029158320252 ) ) ;
#4992 = B_SPLINE_CURVE_WITH_KNOTS ( 'NONE', 3,
 ( #11684, #8483, #14967, #386, #9333, #7403, #15401, #20586, #816, #15716, #5693, #12202, #10933, #9119 ),
 .UNSPECIFIED., .F., .F.,
 ( 4, 2, 2, 2, 2, 2, 4 ),
 ( 0.000000000000000000, 9.722885556680744862E-05, 0.0001944577111336148972, 0.0003889154222671841496, 0.0007778308445342767925, 0.001555661689068462078, 0.003111323378136812267 ),
 .UNSPECIFIED. ) ;
#4993 = CARTESIAN_POINT ( 'NONE',  ( -0.3594811632358368425, 49.16218137147969003, 94.01483168766085896 ) ) ;
#4994 = DIRECTION ( 'NONE',  ( -1.000000000000000000, 1.110223024625156294E-16, 2.267473790562806848E-16 ) ) ;
#4995 = CARTESIAN_POINT ( 'NONE',  ( 5.083341947918205150, 50.97915212978642785, 75.37133819800362744 ) ) ;
#4996 = CARTESIAN_POINT ( 'NONE',  ( -0.5613265744751935182, 49.60399982207104586, 92.45433879953098710 ) ) ;
#4997 = VERTEX_POINT ( 'NONE', #19227 ) ;
#4998 = LINE ( 'NONE', #13208, #20300 ) ;
#4999 = VERTEX_POINT ( 'NONE', #11272 ) ;
#5000 = CARTESIAN_POINT ( 'NONE',  ( 3.460444912181559474, 49.25145096859824889, 90.49246380123798872 ) ) ;
#5001 = EDGE_CURVE ( 'NONE', #11406, #7289, #6454, .T. ) ;
#5002 = VECTOR ( 'NONE', #4870, 1000.000000000000227 ) ;
#5003 = CARTESIAN_POINT ( 'NONE',  ( 1.081950717574418963, 52.20974765063458989, 76.77198585835439815 ) ) ;
#5004 = DIRECTION ( 'NONE',  ( 1.084202172485505420E-16, 1.000000000000000000, 0.000000000000000000 ) ) ;
#5005 = VECTOR ( 'NONE', #17055, 1000.000000000000000 ) ;
#5006 = CARTESIAN_POINT ( 'NONE',  ( -1.403474231502331637, 49.90122385011594019, 75.45433879953087342 ) ) ;
#5007 = ORIENTED_EDGE ( 'NONE', *, *, #591, .T. ) ;
#5008 = CARTESIAN_POINT ( 'NONE',  ( 2.522153740306509739, 50.16218137147969713, 61.15433879953099705 ) ) ;
#5009 = ADVANCED_FACE ( 'NONE', ( #3272 ), #2955, .F. ) ;
#5010 = ORIENTED_EDGE ( 'NONE', *, *, #5982, .T. ) ;
#5011 = CARTESIAN_POINT ( 'NONE',  ( -7.712688300188555779, 47.26501720182910304, 78.14978456997452838 ) ) ;
#5012 = LINE ( 'NONE', #9725, #393 ) ;
#5013 = DIRECTION ( 'NONE',  ( 1.540237394707284220E-16, 1.793354297423764243E-16, -1.000000000000000000 ) ) ;
#5014 = ORIENTED_EDGE ( 'NONE', *, *, #3536, .F. ) ;
#5015 = CARTESIAN_POINT ( 'NONE',  ( 8.253192067227004713, 41.42870919820841635, 77.94607846572662879 ) ) ;
#5016 = CARTESIAN_POINT ( 'NONE',  ( -5.086258153195707621, 37.36447471160525424, 79.53654225555244750 ) ) ;
#5017 = AXIS2_PLACEMENT_3D ( 'NONE', #9278, #5958, #20531 ) ;
#5018 = CARTESIAN_POINT ( 'NONE',  ( 5.904402762709062280, 51.12694543383925350, 76.06909773771320715 ) ) ;
#5019 = CARTESIAN_POINT ( 'NONE',  ( -4.030505877904165146, 50.97787427712486164, 78.52322435057745054 ) ) ;
#5020 = PLANE ( 'NONE',  #7885 ) ;
#5021 = ORIENTED_EDGE ( 'NONE', *, *, #6845, .F. ) ;
#5022 = DIRECTION ( 'NONE',  ( 1.000000000000000000, 1.402518428993831676E-16, 0.000000000000000000 ) ) ;
#5023 = CARTESIAN_POINT ( 'NONE',  ( 5.902048492000326441, 51.12868443877599134, 78.27786821129558348 ) ) ;
#5024 = ORIENTED_EDGE ( 'NONE', *, *, #4151, .T. ) ;
#5025 = CARTESIAN_POINT ( 'NONE',  ( 4.186600743578833494, 51.48180158285643415, 78.06776350345396054 ) ) ;
#5026 = DIRECTION ( 'NONE',  ( 0.000000000000000000, 2.891205793294680792E-16, 1.000000000000000000 ) ) ;
#5027 = DIRECTION ( 'NONE',  ( -0.3165065846431827645, -0.9485903129789529098, 0.000000000000000000 ) ) ;
#5028 = CARTESIAN_POINT ( 'NONE',  ( 2.232254456934871012, 39.46371826755015633, 94.67308879611699979 ) ) ;
#5029 = EDGE_CURVE ( 'NONE', #19138, #18543, #17992, .T. ) ;
#5030 = CARTESIAN_POINT ( 'NONE',  ( -4.622577041588896485, 46.56120873422322859, 93.65746379782397923 ) ) ;
#5031 = CARTESIAN_POINT ( 'NONE',  ( 5.407234661254054942, 37.58402455804959175, 75.99604373986946371 ) ) ;
#5032 = DIRECTION ( 'NONE',  ( 3.154042683594179047E-15, 0.000000000000000000, -1.000000000000000000 ) ) ;
#5033 = VECTOR ( 'NONE', #20559, 1000.000000000000000 ) ;
#5034 = CARTESIAN_POINT ( 'NONE',  ( 5.937214047150960461, 51.10270905974117994, 76.26580079864017137 ) ) ;
#5035 = VERTEX_POINT ( 'NONE', #9777 ) ;
#5036 = CARTESIAN_POINT ( 'NONE',  ( 1.851481395807867747, 48.14626068599128672, 82.45433879953087342 ) ) ;
#5037 = LINE ( 'NONE', #19923, #9576 ) ;
#5038 = VERTEX_POINT ( 'NONE', #17534 ) ;
#5039 = CARTESIAN_POINT ( 'NONE',  ( -2.500166695032101760, 48.49377146048118448, 93.72752763193321357 ) ) ;
#5040 = EDGE_CURVE ( 'NONE', #889, #16595, #19438, .T. ) ;
#5041 = DIRECTION ( 'NONE',  ( 0.000000000000000000, -2.168404344970984808E-15, -1.000000000000000000 ) ) ;
#5042 = CARTESIAN_POINT ( 'NONE',  ( 9.150799720292940975, 42.21925177981464117, 79.41516958226422673 ) ) ;
#5043 = ORIENTED_EDGE ( 'NONE', *, *, #13629, .F. ) ;
#5044 = CARTESIAN_POINT ( 'NONE',  ( 9.539487329945080418, 45.16218137147970424, 73.00433879953099847 ) ) ;
#5045 = CARTESIAN_POINT ( 'NONE',  ( -5.933958468462563474, 37.99063678704128222, 76.24300064276494027 ) ) ;
#5047 = EDGE_CURVE ( 'NONE', #54, #9854, #10963, .T. ) ;
#5046 = ORIENTED_EDGE ( 'NONE', *, *, #14969, .T. ) ;
#5048 = CARTESIAN_POINT ( 'NONE',  ( 2.350558581813038117, 49.87752504164859602, 53.32593395802448555 ) ) ;
#5049 = DIRECTION ( 'NONE',  ( 0.4999999999999984457, 0.8660254037844394848, -0.000000000000000000 ) ) ;
#5050 = FACE_OUTER_BOUND ( 'NONE', #5293, .T. ) ;
#5051 = ORIENTED_EDGE ( 'NONE', *, *, #19143, .T. ) ;
#5052 = DIRECTION ( 'NONE',  ( 1.540237394707284220E-16, 1.793354297423764243E-16, -1.000000000000000000 ) ) ;
#5053 = DIRECTION ( 'NONE',  ( -2.267473790562806355E-16, 5.922860397471811774E-17, -1.000000000000000000 ) ) ;
#5054 = CARTESIAN_POINT ( 'NONE',  ( -4.176309363623031068, 42.45208065485131499, 94.67308879953097289 ) ) ;
#5055 = CIRCLE ( 'NONE', #9494, 0.5999999999999928724 ) ;
#5056 = VERTEX_POINT ( 'NONE', #1477 ) ;
#5057 = CARTESIAN_POINT ( 'NONE',  ( -1.677846259693481556, 47.73989013547935656, 56.15433879953099705 ) ) ;
#5058 = LINE ( 'NONE', #16358, #16223 ) ;
#5059 = CARTESIAN_POINT ( 'NONE',  ( 5.396367158938475406, 37.56735342610807749, 75.36172901897782594 ) ) ;
#5060 = EDGE_CURVE ( 'NONE', #14869, #13044, #2367, .T. ) ;
#5061 =( BOUNDED_CURVE ( )  B_SPLINE_CURVE ( 2, ( #17234, #2661, #16923, #8952, #20204, #750, #4146, #13731, #4037 ),
 .UNSPECIFIED., .F., .F. ) 
 B_SPLINE_CURVE_WITH_KNOTS ( ( 3, 2, 2, 2, 3 ),
 ( 0.2030272526279940093, 0.2083266037756280609, 0.2343674292475841914, 0.2604082547195403219, 0.2851266610854426564 ),
 .UNSPECIFIED. ) 
 CURVE ( )  GEOMETRIC_REPRESENTATION_ITEM ( )  RATIONAL_B_SPLINE_CURVE ( ( 0.9753234597498641190, 0.9845093586922131212, 1.000000000000000000, 0.9238795325112867385, 1.000000000000000000, 0.9238795325112867385, 1.000000000000000000, 0.9277451227429492908, 0.9926614284717510950 ) ) 
 REPRESENTATION_ITEM ( '' )  );
#5062 = EDGE_CURVE ( 'NONE', #18903, #8686, #3054, .T. ) ;
#5063 = EDGE_CURVE ( 'NONE', #12696, #16856, #13486, .T. ) ;
#5064 = CARTESIAN_POINT ( 'NONE',  ( 31.22215374030650281, 42.76218137147968434, 74.20433879953100131 ) ) ;
#5065 = LINE ( 'NONE', #19541, #8235 ) ;
#5066 = EDGE_CURVE ( 'NONE', #11018, #2442, #7963, .T. ) ;
#5067 = CARTESIAN_POINT ( 'NONE',  ( 4.523044550153707988, 37.12507482698154604, 75.49492869865662215 ) ) ;
#5068 = VECTOR ( 'NONE', #11167, 999.9999999999998863 ) ;
#5069 = VERTEX_POINT ( 'NONE', #11063 ) ;
#5070 = CYLINDRICAL_SURFACE ( 'NONE', #16642, 8.799999999999995381 ) ;
#5071 = DIRECTION ( 'NONE',  ( 0.007885122365275663500, 0.9999689119394085113, 1.805443505845543142E-16 ) ) ;
#5072 = LINE ( 'NONE', #4963, #10990 ) ;
#5073 = CARTESIAN_POINT ( 'NONE',  ( 2.101630697682613125, 52.81929183848976805, 78.66284909142584070 ) ) ;
#5074 = ORIENTED_EDGE ( 'NONE', *, *, #7153, .T. ) ;
#5075 = ORIENTED_EDGE ( 'NONE', *, *, #8577, .T. ) ;
#5076 = VECTOR ( 'NONE', #18658, 1000.000000000000227 ) ;
#5077 = CLOSED_SHELL ( 'NONE', ( #11488, #8970, #11188, #12069, #14384, #270, #4796, #7423, #19235, #15491, #7584, #5385, #14392, #20285, #9668, #17148, #470, #15399, #16111, #16878, #6133, #17165, #7914, #17887, #13260, #16278, #1839, #4665, #16394, #18485, #13002, #16611, #7455, #9478, #11019, #9617, #18507, #9594, #3884, #16098, #10145, #2700, #15361, #12986, #12594, #18710, #15758, #2315, #7961, #11061, #5697, #18318, #16921, #2209, #17297, #3078, #18473, #4449, #20935, #13395, #7221, #12859, #20024, #12619, #8761, #18172, #18683, #1984, #7669, #14270, #4565, #8853, #7811, #3454, #11938, #11721, #7566, #10125, #12125, #15712, #7369, #16396, #3419, #6846, #6921, #5265, #16671, #20926, #2866, #7902, #1447, #7273, #10032, #14903, #16280, #5304, #15745, #15511, #15864, #12840, #18142, #18354, #10796, #14934, #18124, #18059 ) ) ;
#5078 = DIRECTION ( 'NONE',  ( 1.000000000000000000, -0.000000000000000000, -0.000000000000000000 ) ) ;
#5079 = ORIENTED_EDGE ( 'NONE', *, *, #7004, .F. ) ;
#5080 = VECTOR ( 'NONE', #3339, 1000.000000000000000 ) ;
#5081 = CARTESIAN_POINT ( 'NONE',  ( 6.876224750190004897, 50.40909967906462441, 75.93520998463665705 ) ) ;
#5082 = CARTESIAN_POINT ( 'NONE',  ( 9.353743827924017040, 42.82748814491910139, 76.70850639745313515 ) ) ;
#5083 = CARTESIAN_POINT ( 'NONE',  ( -0.9074515375185698840, 52.84529689527732899, 76.19569360893534338 ) ) ;
#5084 = CARTESIAN_POINT ( 'NONE',  ( 2.463659247115867146, 38.82793883177424732, 92.87621379782399345 ) ) ;
#5085 = VECTOR ( 'NONE', #9032, 1000.000000000000000 ) ;
#5086 = PLANE ( 'NONE',  #11492 ) ;
#5087 = AXIS2_PLACEMENT_3D ( 'NONE', #10496, #10390, #16859 ) ;
#5088 = CARTESIAN_POINT ( 'NONE',  ( 4.575658464751415799, 52.10843532165534953, 76.08931382966170531 ) ) ;
#5089 = CARTESIAN_POINT ( 'NONE',  ( 8.617444985878929486, 45.46842246209711647, 78.98986195196137317 ) ) ;
#5090 = CARTESIAN_POINT ( 'NONE',  ( 8.385679600361122255, 39.92613824206362949, 77.13595644658970230 ) ) ;
#5091 = ADVANCED_FACE ( 'NONE', ( #6347 ), #15995, .T. ) ;
#5092 = CARTESIAN_POINT ( 'NONE',  ( 5.611423337425062385, 41.22389019960463230, 93.92996380123798872 ) ) ;
#5093 = ORIENTED_EDGE ( 'NONE', *, *, #18272, .F. ) ;
#5094 = EDGE_CURVE ( 'NONE', #667, #17901, #20005, .T. ) ;
#5095 = CARTESIAN_POINT ( 'NONE',  ( 0.4418570709954666720, 52.35535905447424199, 75.99769453967874711 ) ) ;
#5096 = LINE ( 'NONE', #11615, #4786 ) ;
#5097 = CARTESIAN_POINT ( 'NONE',  ( 2.522153740306511960, 47.62628298661745418, 45.55433879953100273 ) ) ;
#5098 = VECTOR ( 'NONE', #10220, 1000.000000000000000 ) ;
#5099 = CARTESIAN_POINT ( 'NONE',  ( 27.03948732994508930, 43.16218137147969003, 78.30433879953100984 ) ) ;
#5100 = CARTESIAN_POINT ( 'NONE',  ( 9.155505153612395475, 42.23335426198017473, 78.07975471416389723 ) ) ;
#5101 = ORIENTED_EDGE ( 'NONE', *, *, #7430, .F. ) ;
#5102 = CIRCLE ( 'NONE', #8167, 1.399999999999995026 ) ;
#5103 = CARTESIAN_POINT ( 'NONE',  ( 0.6392524745555471233, 52.20500180601669626, 79.54845644658969661 ) ) ;
#5104 = CARTESIAN_POINT ( 'NONE',  ( 7.696648035528455445, 40.19142276524996760, 78.71587240337095182 ) ) ;
#5105 = DIRECTION ( 'NONE',  ( 0.3015081906286226077, -0.9534635866061452747, -1.245503830460468341E-16 ) ) ;
#5106 = DIRECTION ( 'NONE',  ( -0.000000000000000000, 0.000000000000000000, -1.000000000000000000 ) ) ;
#5107 = ORIENTED_EDGE ( 'NONE', *, *, #2468, .F. ) ;
#5108 = CARTESIAN_POINT ( 'NONE',  ( 8.375126220672854060, 41.81456477263208882, 76.36070165242202279 ) ) ;
#5109 = LINE ( 'NONE', #15338, #7480 ) ;
#5110 = ORIENTED_EDGE ( 'NONE', *, *, #9388, .T. ) ;
#5111 = CARTESIAN_POINT ( 'NONE',  ( 4.394343283833276992, 39.11584570990505938, 91.35183880123798872 ) ) ;
#5112 = CARTESIAN_POINT ( 'NONE',  ( -7.783762692441060338, 41.22945570740913723, 78.68823452940202401 ) ) ;
#5113 = CARTESIAN_POINT ( 'NONE',  ( -4.524181921268124462, 40.28999182795290324, 94.78933880123798872 ) ) ;
#5114 = CARTESIAN_POINT ( 'NONE',  ( 8.530649028577993676, 48.02340768410154936, 78.56977997600147035 ) ) ;
#5115 = EDGE_LOOP ( 'NONE', ( #7492, #1098, #2522, #11641 ) ) ;
#5116 = DIRECTION ( 'NONE',  ( -0.5773502691896219563, 0.5773502691896226224, -0.5773502691896327255 ) ) ;
#5117 = VERTEX_POINT ( 'NONE', #8699 ) ;
#5118 = FACE_OUTER_BOUND ( 'NONE', #18194, .T. ) ;
#5119 = CARTESIAN_POINT ( 'NONE',  ( 3.460444912181559474, 49.25145096859824889, 90.64871380123798872 ) ) ;
#5120 = AXIS2_PLACEMENT_3D ( 'NONE', #14736, #6743, #1964 ) ;
#5121 = LINE ( 'NONE', #14498, #15948 ) ;
#5122 = VERTEX_POINT ( 'NONE', #6875 ) ;
#5123 = CARTESIAN_POINT ( 'NONE',  ( -1.392380047608623883, 49.84925249003585179, 77.23980501161587142 ) ) ;
#5124 = DIRECTION ( 'NONE',  ( -1.193617070626243484E-16, -1.000000000000000000, -0.000000000000000000 ) ) ;
#5125 = CARTESIAN_POINT ( 'NONE',  ( 31.07218010054375412, 42.96218137147968008, 65.80574467885102763 ) ) ;
#5126 = DIRECTION ( 'NONE',  ( -1.334402673828313339E-16, 1.592765810570777996E-32, 1.000000000000000000 ) ) ;
#5127 = CARTESIAN_POINT ( 'NONE',  ( 0.4713596985539078577, 52.96647961732049481, 78.91893668031715947 ) ) ;
#5128 = ORIENTED_EDGE ( 'NONE', *, *, #15102, .T. ) ;
#5129 = CARTESIAN_POINT ( 'NONE',  ( -4.392497846706504561, 51.46612350181082007, 76.19049300047602458 ) ) ;
#5130 = VERTEX_POINT ( 'NONE', #5270 ) ;
#5131 = DIRECTION ( 'NONE',  ( -1.110223024625156540E-16, -1.000000000000000000, -5.922860397471808077E-17 ) ) ;
#5132 = CARTESIAN_POINT ( 'NONE',  ( -7.508333715179515977, 40.35369624421328183, 77.67144260532384692 ) ) ;
#5133 = CARTESIAN_POINT ( 'NONE',  ( -4.792503378000012582, 37.91763016944491227, 77.33669174070733732 ) ) ;
#5134 = CARTESIAN_POINT ( 'NONE',  ( 5.220616844236031007, 45.87228208810806507, 93.73558879611698558 ) ) ;
#5135 = VECTOR ( 'NONE', #713, 1000.000000000000000 ) ;
#5136 = CARTESIAN_POINT ( 'NONE',  ( 0.2541436421823703995, 38.02374091943176637, 94.04808879782397923 ) ) ;
#5137 = CARTESIAN_POINT ( 'NONE',  ( 5.824901997307729395, 37.13555891239614226, 76.06531707679772580 ) ) ;
#5138 = CIRCLE ( 'NONE', #2108, 6.000000000000002665 ) ;
#5139 = CARTESIAN_POINT ( 'NONE',  ( 2.522153740306506631, 49.16218137147969003, 74.55433879953100984 ) ) ;
#5140 = VERTEX_POINT ( 'NONE', #493 ) ;
#5141 = DIRECTION ( 'NONE',  ( -1.540237394707284220E-16, -1.793354297423764243E-16, 1.000000000000000000 ) ) ;
#5142 = LINE ( 'NONE', #9851, #17713 ) ;
#5143 = ORIENTED_EDGE ( 'NONE', *, *, #2750, .T. ) ;
#5144 = CARTESIAN_POINT ( 'NONE',  ( -5.838428831739582492, 50.43291415881836315, 76.76022115247205591 ) ) ;
#5145 = ADVANCED_FACE ( 'NONE', ( #6970 ), #13474, .T. ) ;
#5146 = PLANE ( 'NONE',  #11288 ) ;
#5147 = CARTESIAN_POINT ( 'NONE',  ( -4.500660556396669065, 42.81632233694663370, 92.75808879953098085 ) ) ;
#5148 = EDGE_LOOP ( 'NONE', ( #1201, #7062, #11274, #20752 ) ) ;
#5149 = CARTESIAN_POINT ( 'NONE',  ( -4.501441463659942244, 37.86850067699155886, 75.36972643424059015 ) ) ;
#5150 = ORIENTED_EDGE ( 'NONE', *, *, #11988, .F. ) ;
#5151 = AXIS2_PLACEMENT_3D ( 'NONE', #8834, #17020, #4343 ) ;
#5152 = DIRECTION ( 'NONE',  ( 1.000000000000000000, -1.110223024625156540E-16, 1.779391786395883043E-16 ) ) ;
#5153 = LINE ( 'NONE', #8581, #2704 ) ;
#5154 = CARTESIAN_POINT ( 'NONE',  ( 5.025485839985549319, 41.56218137147963887, 94.47683879953099506 ) ) ;
#5155 = AXIS2_PLACEMENT_3D ( 'NONE', #20122, #20551, #15566 ) ;
#5156 = VERTEX_POINT ( 'NONE', #4958 ) ;
#5157 = DIRECTION ( 'NONE',  ( 3.154042683594179442E-15, -3.469446951953613203E-16, -1.000000000000000000 ) ) ;
#5158 = VERTEX_POINT ( 'NONE', #2199 ) ;
#5159 = LINE ( 'NONE', #16462, #13495 ) ;
#5160 = LINE ( 'NONE', #19636, #18346 ) ;
#5161 = EDGE_CURVE ( 'NONE', #20489, #10457, #4056, .T. ) ;
#5162 = CARTESIAN_POINT ( 'NONE',  ( 5.956380690854414794, 50.16371848513034593, 75.46588380158773646 ) ) ;
#5163 = CARTESIAN_POINT ( 'NONE',  ( 5.848951923618479931, 37.15274410921379911, 76.58742703482498371 ) ) ;
#5164 = VECTOR ( 'NONE', #4209, 1000.000000000000000 ) ;
#5165 = CARTESIAN_POINT ( 'NONE',  ( -4.307690844420870135, 37.53294895003197951, 79.54647054202554557 ) ) ;
#5166 = CARTESIAN_POINT ( 'NONE',  ( 5.378304226687590450, 36.81643649649897299, 75.37835156746757548 ) ) ;
#5167 = VECTOR ( 'NONE', #13291, 1000.000000000000114 ) ;
#5168 = EDGE_CURVE ( 'NONE', #18997, #15510, #13790, .T. ) ;
#5169 = CARTESIAN_POINT ( 'NONE',  ( 7.678973061664008171, 40.17251196347450559, 78.40165754912887053 ) ) ;
#5170 = ORIENTED_EDGE ( 'NONE', *, *, #10100, .F. ) ;
#5171 = CARTESIAN_POINT ( 'NONE',  ( -0.9271010316932370987, 52.23309654930653778, 78.54091960784487014 ) ) ;
#5172 = CARTESIAN_POINT ( 'NONE',  ( 8.637025618647824032, 43.04385625447593355, 76.23134092453109645 ) ) ;
#5173 = DIRECTION ( 'NONE',  ( 0.5670994908670485835, -0.8236492988270761595, -6.036271672687166828E-17 ) ) ;
#5174 = CARTESIAN_POINT ( 'NONE',  ( 4.394343283833276992, 39.11584570990505938, 94.00808880123797451 ) ) ;
#5175 = APPLICATION_CONTEXT ( 'automotive_design' ) ;
#5176 = ADVANCED_FACE ( 'NONE', ( #9122 ), #12763, .F. ) ;
#5177 = ORIENTED_EDGE ( 'NONE', *, *, #2877, .F. ) ;
#5178 = EDGE_CURVE ( 'NONE', #6135, #7903, #10631, .T. ) ;
#5179 = ORIENTED_EDGE ( 'NONE', *, *, #13683, .F. ) ;
#5180 = CARTESIAN_POINT ( 'NONE',  ( 5.542130322670880460, 50.64142601547018785, 78.59183879953087626 ) ) ;
#5181 = ORIENTED_EDGE ( 'NONE', *, *, #18553, .T. ) ;
#5182 = CARTESIAN_POINT ( 'NONE',  ( 5.522356516757287892, 50.66127187491098027, 76.02767501797669070 ) ) ;
#5183 = CARTESIAN_POINT ( 'NONE',  ( 9.162426004170315608, 42.25409649015283975, 75.50722976489458915 ) ) ;
#5184 = DIRECTION ( 'NONE',  ( -0.5800177190770277047, -0.8146038580541355989, -2.354238310054624259E-16 ) ) ;
#5185 = EDGE_CURVE ( 'NONE', #188, #17910, #6093, .T. ) ;
#5186 = DIRECTION ( 'NONE',  ( -1.540237394707284220E-16, -1.793354297423764243E-16, 1.000000000000000000 ) ) ;
#5187 = DIRECTION ( 'NONE',  ( 0.007885122365278605591, 0.9999689119394085113, 1.805443505845548073E-16 ) ) ;
#5188 = CARTESIAN_POINT ( 'NONE',  ( 0.8460310913591665427, 52.96352569016541878, 77.64755553332491900 ) ) ;
#5189 = CARTESIAN_POINT ( 'NONE',  ( 5.901851037876958195, 51.12883029018298231, 78.62249727093715990 ) ) ;
#5190 = CARTESIAN_POINT ( 'NONE',  ( 4.732847133705871734, 51.99232638384451377, 75.72008365543779007 ) ) ;
#5191 = CARTESIAN_POINT ( 'NONE',  ( -5.784195910403845176, 44.99242805365518194, 92.13308880123798872 ) ) ;
#5192 = CARTESIAN_POINT ( 'NONE',  ( -5.784195910403845176, 44.99242805365518194, 90.88308880123798872 ) ) ;
#5193 = ORIENTED_EDGE ( 'NONE', *, *, #16267, .T. ) ;
#5194 = CARTESIAN_POINT ( 'NONE',  ( 30.92220646078100188, 42.76218137147968434, 58.20715055817105110 ) ) ;
#5195 = AXIS2_PLACEMENT_3D ( 'NONE', #13513, #14508, #19502 ) ;
#5196 = CARTESIAN_POINT ( 'NONE',  ( -5.835675398032521777, 50.43488166173578691, 78.31711373209397209 ) ) ;
#5197 = CARTESIAN_POINT ( 'NONE',  ( -4.519331755718375199, 37.70034496097993326, 78.77850703318271997 ) ) ;
#5198 = EDGE_CURVE ( 'NONE', #6491, #13246, #9431, .T. ) ;
#5199 = CARTESIAN_POINT ( 'NONE',  ( -1.219503646467433589, 49.90383875825363447, 77.41268141275706682 ) ) ;
#5200 = DIRECTION ( 'NONE',  ( 5.626130192357176673E-16, 1.831515347669941892E-30, -1.000000000000000000 ) ) ;
#5201 = EDGE_CURVE ( 'NONE', #2164, #19006, #4416, .T. ) ;
#5202 = CARTESIAN_POINT ( 'NONE',  ( -4.500660556396669065, 42.81632233694663370, 93.07058880294496817 ) ) ;
#5203 = ORIENTED_EDGE ( 'NONE', *, *, #10660, .F. ) ;
#5204 = VERTEX_POINT ( 'NONE', #14417 ) ;
#5205 = CARTESIAN_POINT ( 'NONE',  ( 6.104265285658651230, 38.25495727238729415, 78.24541959536460922 ) ) ;
#5206 = CARTESIAN_POINT ( 'NONE',  ( -3.495065479208315562, 36.18912478048144266, 76.62933879953087057 ) ) ;
#5207 = ADVANCED_FACE ( 'NONE', ( #2832 ), #4762, .F. ) ;
#5208 = CARTESIAN_POINT ( 'NONE',  ( 0.6901636094616421246, 52.96072213236104176, 75.98019638678815113 ) ) ;
#5209 = VERTEX_POINT ( 'NONE', #5244 ) ;
#5210 = CARTESIAN_POINT ( 'NONE',  ( -4.427139072037590495, 51.44137015048543304, 78.85744209785094938 ) ) ;
#5211 = EDGE_CURVE ( 'NONE', #2305, #7517, #1695, .T. ) ;
#5212 = VECTOR ( 'NONE', #8182, 1000.000000000000114 ) ;
#5213 = CARTESIAN_POINT ( 'NONE',  ( -4.539440361571185356, 36.96056243609647396, 78.81995494622690046 ) ) ;
#5214 = VERTEX_POINT ( 'NONE', #18236 ) ;
#5215 = CARTESIAN_POINT ( 'NONE',  ( -3.943187491250720544, 40.73580453397070755, 94.39871380294496817 ) ) ;
#5216 = CARTESIAN_POINT ( 'NONE',  ( 2.120143825079129574, 52.94022564282578003, 77.78911287202200242 ) ) ;
#5217 = CARTESIAN_POINT ( 'NONE',  ( -4.524181921268124462, 40.28999182795290324, 92.28933880123798872 ) ) ;
#5218 = CARTESIAN_POINT ( 'NONE',  ( -5.154188915835984375, 42.64120994080404614, 91.11746380123797451 ) ) ;
#5219 = B_SPLINE_CURVE_WITH_KNOTS ( 'NONE', 3,
 ( #13781, #12194, #20481, #15813, #9009, #4203, #17091, #9223, #12308, #9112, #4510, #15599, #2612, #14195, #17189, #7715, #12411, #2514 ),
 .UNSPECIFIED., .F., .F.,
 ( 4, 2, 2, 2, 2, 2, 2, 2, 4 ),
 ( 8.673617379884035472E-19, 0.0003077246462501492027, 0.0006154492925002975380, 0.0009231739387504458733, 0.001230898585000594209, 0.001538623231250742544, 0.001846347877500890879, 0.002154072523751038998, 0.002461797170001187550 ),
 .UNSPECIFIED. ) ;
#5220 = CARTESIAN_POINT ( 'NONE',  ( 8.121917471046002035, 44.10225444150351137, 75.45433879953087342 ) ) ;
#5221 = EDGE_LOOP ( 'NONE', ( #9651, #13606, #10412, #918 ) ) ;
#5222 = CARTESIAN_POINT ( 'NONE',  ( -4.383473025373059606, 51.47257230871590394, 78.45066232894264147 ) ) ;
#5223 = VERTEX_POINT ( 'NONE', #16447 ) ;
#5224 = LINE ( 'NONE', #13432, #8163 ) ;
#5225 = CARTESIAN_POINT ( 'NONE',  ( 5.568489401881125289, 48.03437091500646261, 95.41433880123797451 ) ) ;
#5226 = ORIENTED_EDGE ( 'NONE', *, *, #915, .T. ) ;
#5227 = B_SPLINE_CURVE_WITH_KNOTS ( 'NONE', 3,
 ( #2606, #15388, #13561, #12405, #3876, #7287, #579, #5471, #5678, #18667, #5797, #10723, #17183, #10503, #7061 ),
 .UNSPECIFIED., .F., .F.,
 ( 4, 1, 1, 1, 1, 1, 1, 1, 1, 1, 1, 1, 4 ),
 ( 0.000000000000000000, 0.1198978896105060005, 0.2272848286615199442, 0.3233685559759303385, 0.4081414772668706115, 0.4819378103613651820, 0.5435227337441967954, 0.5948163272532476231, 0.6357474925148977052, 0.7079723711143988130, 0.7877128652614201476, 0.8832591045952046249, 1.000000000000000000 ),
 .UNSPECIFIED. ) ;
#5228 = CARTESIAN_POINT ( 'NONE',  ( -6.613032277150673544, 45.52591812603678534, 75.45433879953087342 ) ) ;
#5229 = CARTESIAN_POINT ( 'NONE',  ( 8.707758170209565662, 40.89142814818289651, 75.40210940951681096 ) ) ;
#5230 = CARTESIAN_POINT ( 'NONE',  ( -4.689916854477828245, 37.07171335984372718, 78.93589701864812014 ) ) ;
#5231 = CARTESIAN_POINT ( 'NONE',  ( 0.3326973149608342673, 52.96014171822455552, 72.45433879953087342 ) ) ;
#5232 = EDGE_CURVE ( 'NONE', #502, #19108, #6779, .T. ) ;
#5233 = CARTESIAN_POINT ( 'NONE',  ( 0.3328022465261254448, 52.96757219375044201, 78.52223653336807274 ) ) ;
#5234 = EDGE_LOOP ( 'NONE', ( #7443, #19106, #8522, #10518 ) ) ;
#5235 = CARTESIAN_POINT ( 'NONE',  ( -3.116943990436417788, 39.65933899544464225, 92.55433879953100984 ) ) ;
#5236 = ORIENTED_EDGE ( 'NONE', *, *, #6503, .F. ) ;
#5237 = CARTESIAN_POINT ( 'NONE',  ( -3.304399724198308519, 36.90940894797284955, 77.85413967038655869 ) ) ;
#5238 = CARTESIAN_POINT ( 'NONE',  ( -6.731127884703168363, 40.37999424897662948, 78.06261470525505786 ) ) ;
#5239 = CARTESIAN_POINT ( 'NONE',  ( -4.646812029368017072, 37.79580252097101578, 77.33278042858304957 ) ) ;
#5240 = CARTESIAN_POINT ( 'NONE',  ( 0.2860873169776713132, 38.75537135769874197, 92.09496379611698558 ) ) ;
#5241 = CARTESIAN_POINT ( 'NONE',  ( -1.419351766502867429, 49.49642391118513274, 92.40746379782397923 ) ) ;
#5242 = CARTESIAN_POINT ( 'NONE',  ( 5.846647460608473956, 37.15109742431862827, 76.40678776405631822 ) ) ;
#5243 = EDGE_LOOP ( 'NONE', ( #5107, #7114, #16867, #4705 ) ) ;
#5244 = CARTESIAN_POINT ( 'NONE',  ( -4.249412910294118717, 50.83092575845958550, 78.93669174070734584 ) ) ;
#5245 = CARTESIAN_POINT ( 'NONE',  ( -7.677846259693480668, 38.96218137147968008, 93.55433879953098142 ) ) ;
#5246 = VERTEX_POINT ( 'NONE', #9850 ) ;
#5247 = LINE ( 'NONE', #5144, #15651 ) ;
#5248 = EDGE_CURVE ( 'NONE', #3162, #8103, #16648, .T. ) ;
#5249 = FACE_OUTER_BOUND ( 'NONE', #1326, .T. ) ;
#5250 = CARTESIAN_POINT ( 'NONE',  ( -5.058133621542618030, 44.89684013992257405, 93.92996379953099506 ) ) ;
#5251 = VERTEX_POINT ( 'NONE', #8354 ) ;
#5252 = LINE ( 'NONE', #13148, #19052 ) ;
#5253 = CARTESIAN_POINT ( 'NONE',  ( -5.056163503743588805, 37.34224500634140043, 75.38158877174898009 ) ) ;
#5254 = ORIENTED_EDGE ( 'NONE', *, *, #13035, .T. ) ;
#5255 = FACE_OUTER_BOUND ( 'NONE', #19209, .T. ) ;
#5256 = CARTESIAN_POINT ( 'NONE',  ( 0.5311529524219201770, 52.96235922873796653, 76.89393617185528740 ) ) ;
#5257 = ORIENTED_EDGE ( 'NONE', *, *, #16533, .T. ) ;
#5258 = CARTESIAN_POINT ( 'NONE',  ( -4.753731435370094793, 37.11885062014069092, 77.91594000873737969 ) ) ;
#5259 = CARTESIAN_POINT ( 'NONE',  ( -4.524181921268124462, 40.28999182795290324, 96.19558880123798872 ) ) ;
#5260 = ORIENTED_EDGE ( 'NONE', *, *, #12972, .T. ) ;
#5261 = CARTESIAN_POINT ( 'NONE',  ( 0.8256759245549851745, 52.35658408014969467, 77.54407321495646954 ) ) ;
#5262 = CARTESIAN_POINT ( 'NONE',  ( 0.7793394610543057377, 52.95888126071579904, 75.36251995630715328 ) ) ;
#5263 = CARTESIAN_POINT ( 'NONE',  ( 0.000000000000000000, 0.000000000000000000, 0.000000000000000000 ) ) ;
#5264 = CARTESIAN_POINT ( 'NONE',  ( 5.547294332158212882, 50.64200668057274157, 77.20373336814266452 ) ) ;
#5265 = ADVANCED_FACE ( 'NONE', ( #8137 ), #6637, .T. ) ;
#5266 = B_SPLINE_CURVE_WITH_KNOTS ( 'NONE', 3,
 ( #1719, #4884, #11303, #14476, #20942, #3202, #5100, #11618, #3515, #4988, #19467, #9, #14581, #10018, #310, #6483, #6376, #11405, #9804, #2807, #4589, #2696, #2910 ),
 .UNSPECIFIED., .F., .F.,
 ( 4, 1, 1, 1, 1, 1, 1, 1, 1, 1, 1, 1, 1, 1, 1, 1, 1, 1, 1, 1, 4 ),
 ( 0.000000000000000000, 0.05038957832574614271, 0.09924218466120336701, 0.1466944942679149211, 0.1933274803506509210, 0.2393051970681265017, 0.2845336341364397836, 0.3290963736026611408, 0.3737734709422849688, 0.4170414937111141529, 0.4581341819676884586, 0.4966705307863439889, 0.5335170563061359950, 0.5686625127317078698, 0.6026561223054673899, 0.6353294289861355360, 0.6676748031221235724, 0.7363421380907280156, 0.8138933404431207830, 0.9017813486866357309, 1.000000000000000000 ),
 .UNSPECIFIED. ) ;
#5267 = DIRECTION ( 'NONE',  ( 0.009567942452863074584, -0.9999542261909885044, -1.778535306010356147E-16 ) ) ;
#5268 = VERTEX_POINT ( 'NONE', #1767 ) ;
#5269 = ORIENTED_EDGE ( 'NONE', *, *, #12803, .F. ) ;
#5270 = CARTESIAN_POINT ( 'NONE',  ( -5.838428831739582492, 50.43291415881836315, 76.76022115247205591 ) ) ;
#5271 = CARTESIAN_POINT ( 'NONE',  ( 7.748486061697145821, 40.38084683439631561, 79.09910503406773330 ) ) ;
#5272 = ORIENTED_EDGE ( 'NONE', *, *, #3138, .F. ) ;
#5273 = CARTESIAN_POINT ( 'NONE',  ( -0.9424882101290802394, 52.23031780077558039, 78.01134710528980065 ) ) ;
#5274 = DIRECTION ( 'NONE',  ( -0.9534635866061452747, -0.3015081906286225522, -2.009271279954815797E-16 ) ) ;
#5275 = CARTESIAN_POINT ( 'NONE',  ( -4.524181921268124462, 40.28999182795290324, 93.69558880123800293 ) ) ;
#5276 = ORIENTED_EDGE ( 'NONE', *, *, #16254, .T. ) ;
#5277 = ADVANCED_FACE ( 'NONE', ( #18030 ), #14627, .T. ) ;
#5278 = EDGE_LOOP ( 'NONE', ( #18270, #1609, #12501, #11463 ) ) ;
#5279 = EDGE_CURVE ( 'NONE', #14483, #9281, #7101, .T. ) ;
#5280 = DIRECTION ( 'NONE',  ( -1.000000000000000000, 1.193617070626243484E-16, 0.000000000000000000 ) ) ;
#5281 = VERTEX_POINT ( 'NONE', #16754 ) ;
#5282 = DIRECTION ( 'NONE',  ( -1.000000000000000000, 1.110223024625156540E-16, -1.779391786395883043E-16 ) ) ;
#5283 = CARTESIAN_POINT ( 'NONE',  ( 9.064651367107570579, 41.96105970016846243, 75.41143022427675646 ) ) ;
#5284 = DIRECTION ( 'NONE',  ( -0.5941461771851691553, -0.8043570849667760481, -2.357623395011396791E-16 ) ) ;
#5285 = CARTESIAN_POINT ( 'NONE',  ( -7.376743071288316855, 41.96049357349896525, 72.45433879953085921 ) ) ;
#5286 = CARTESIAN_POINT ( 'NONE',  ( 2.522153740306507519, 47.62628298661744708, 69.15433879953098995 ) ) ;
#5287 = B_SPLINE_SURFACE_WITH_KNOTS ( 'NONE', 3, 1, ( 
 ( #20931, #19150 ),
 ( #6263, #17765 ),
 ( #19246, #1706 ),
 ( #14572, #4561 ),
 ( #4978, #11083 ),
 ( #14674, #99 ),
 ( #6367, #4872 ),
 ( #1598, #2973 ),
 ( #19558, #12867 ),
 ( #12765, #19349 ),
 ( #15965, #11182 ),
 ( #9479, #11499 ),
 ( #20837, #8080 ),
 ( #4767, #3192 ),
 ( #16175, #14983 ) ),
 .UNSPECIFIED., .F., .F., .F.,
 ( 4, 1, 1, 1, 1, 1, 1, 1, 1, 1, 1, 1, 4 ),
 ( 2, 2 ),
 ( 0.000000000000000000, 0.1372453196419673171, 0.2656077965333414337, 0.3855481208555507355, 0.4976308828580581767, 0.5516434046647483713, 0.6057582083304485776, 0.6621535423365251249, 0.7211227168729713588, 0.7835375577407022174, 0.8505035567791932039, 0.9228138635028276804, 1.000000000000000000 ),
 ( 0.000000000000000000, 1.000000000000000000 ),
 .UNSPECIFIED. ) ;
#5288 = CARTESIAN_POINT ( 'NONE',  ( 8.221537414170169811, 41.35424937605134943, 76.10950202369875228 ) ) ;
#5289 = DIRECTION ( 'NONE',  ( -0.5954989751681698529, 0.8033560671169786005, 5.234922652618075161E-17 ) ) ;
#5290 = CARTESIAN_POINT ( 'NONE',  ( 4.611425380024144260, 52.08201574212262130, 75.94315254166910734 ) ) ;
#5291 = CARTESIAN_POINT ( 'NONE',  ( -4.500660556396669065, 42.81632233694663370, 95.57058880294496817 ) ) ;
#5292 = CARTESIAN_POINT ( 'NONE',  ( 28.52215374030649642, 47.36218137147967155, 87.05433879953100984 ) ) ;
#5293 = EDGE_LOOP ( 'NONE', ( #10389, #11736, #240, #1910 ) ) ;
#5294 = CARTESIAN_POINT ( 'NONE',  ( 0.3284214782166970936, 52.35625353581157526, 76.35041178738960355 ) ) ;
#5295 = AXIS2_PLACEMENT_3D ( 'NONE', #17364, #17669, #7784 ) ;
#5296 = ORIENTED_EDGE ( 'NONE', *, *, #3595, .F. ) ;
#5297 = LINE ( 'NONE', #17894, #6085 ) ;
#5298 = DIRECTION ( 'NONE',  ( 1.000000000000000000, -0.000000000000000000, -0.000000000000000000 ) ) ;
#5299 = CARTESIAN_POINT ( 'NONE',  ( -2.083470957239372368, 47.45622447009557021, 79.40903933791013003 ) ) ;
#5300 = CARTESIAN_POINT ( 'NONE',  ( 1.352400422481993658, 50.46853102219002096, 91.97683880123797451 ) ) ;
#5301 =( BOUNDED_SURFACE ( )  B_SPLINE_SURFACE ( 1, 2, ( 
 ( #9726, #1631, #14606, #1847, #6826, #8331, #11531, #13332, #19804, #5225, #8012, #11742, #16626, #14810, #20966, #18216, #6401, #231, #12908, #4805, #16207, #133, #11427, #4906, #8116, #6510, #6610, #13017, #19491, #17900, #3322, #9827, #6929, #20115, #16837, #20215, #5648, #18637, #3845, #447, #15352, #18316, #7139, #8655, #2475, #13433, #547, #8866, #19904, #12157, #7249, #20001, #15137, #5328, #11841, #15242, #17050, #2048, #13845, #20325, #7030, #8544, #15031, #13529, #766, #3737, #8968, #10367, #4165, #10258, #5436, #8754, #16733, #13745, #7354, #11952, #5761, #5551, #15453 ),
 ( #2156, #10472, #4052, #12268, #10580, #18750, #18428, #869, #2255, #658, #2362, #13640, #10688, #12056, #18534, #3948, #16936, #19063, #9179, #2889, #7677, #15978, #15670, #18848, #4571, #5968, #2674, #12571, #1090, #12373, #1192, #1290, #14154, #12468, #14060, #974, #7577, #9070, #2789, #7464, #11093, #5875, #17252, #15559, #7886, #2985, #4473, #9491, #12679, #10994, #4260, #1395, #17151, #2572, #18950, #14259, #20544, #19159, #17561, #10786, #4362, #10888, #17465, #7778, #9389, #14372, #20847, #9290, #13960, #15778, #17359, #20442, #20638, #15873, #6067, #20740, #6175, #6274, #12776 ) ),
 .UNSPECIFIED., .F., .F., .F. ) 
 B_SPLINE_SURFACE_WITH_KNOTS ( ( 2, 2 ),
 ( 3, 2, 2, 2, 2, 2, 2, 2, 2, 2, 2, 2, 2, 2, 2, 2, 2, 2, 2, 2, 2, 2, 2, 2, 2, 2, 2, 2, 2, 2, 2, 2, 2, 2, 2, 2, 2, 2, 2, 3 ),
 ( 0.000000000000000000, 1.000000000000000000 ),
 ( 0.000000000000000000, 0.02500000000000000139, 0.05000000000000000278, 0.07499999999999999722, 0.1000000000000000056, 0.1250000000000000000, 0.1499999999999999944, 0.1749999999999999889, 0.2000000000000000111, 0.2250000000000000056, 0.2500000000000000000, 0.2750000000000000222, 0.2999999999999999889, 0.3250000000000000111, 0.3499999999999999778, 0.3750000000000000000, 0.4000000000000000222, 0.4249999999999999889, 0.4500000000000000111, 0.4749999999999999778, 0.5000000000000000000, 0.5250000000000000222, 0.5500000000000000444, 0.5749999999999999556, 0.5999999999999999778, 0.6250000000000000000, 0.6500000000000000222, 0.6750000000000000444, 0.6999999999999999556, 0.7249999999999999778, 0.7500000000000000000, 0.7750000000000000222, 0.8000000000000000444, 0.8249999999999999556, 0.8499999999999999778, 0.8750000000000000000, 0.9000000000000000222, 0.9250000000000000444, 0.9499999999999999556, 0.9600309957089442348 ),
 .UNSPECIFIED. ) 
 GEOMETRIC_REPRESENTATION_ITEM ( )  RATIONAL_B_SPLINE_SURFACE ( (
 ( 1.000000000000000000, 0.9238795325112867385, 1.000000000000000000, 0.9238795325112867385, 1.000000000000000000, 0.9238795325112867385, 1.000000000000000000, 0.9238795325112867385, 1.000000000000000000, 0.9238795325112867385, 1.000000000000000000, 0.9238795325112867385, 1.000000000000000000, 0.9238795325112867385, 1.000000000000000000, 0.9238795325112867385, 1.000000000000000000, 0.9238795325112867385, 1.000000000000000000, 0.9238795325112867385, 1.000000000000000000, 0.9238795325112867385, 1.000000000000000000, 0.9238795325112867385, 1.000000000000000000, 0.9238795325112867385, 1.000000000000000000, 0.9238795325112867385, 1.000000000000000000, 0.9238795325112867385, 1.000000000000000000, 0.9238795325112867385, 1.000000000000000000, 0.9238795325112867385, 1.000000000000000000, 0.9238795325112867385, 1.000000000000000000, 0.9238795325112867385, 1.000000000000000000, 0.9238795325112867385, 1.000000000000000000, 0.9238795325112867385, 1.000000000000000000, 0.9238795325112867385, 1.000000000000000000, 0.9238795325112867385, 1.000000000000000000, 0.9238795325112867385, 1.000000000000000000, 0.9238795325112867385, 1.000000000000000000, 0.9238795325112867385, 1.000000000000000000, 0.9238795325112867385, 1.000000000000000000, 0.9238795325112867385, 1.000000000000000000, 0.9238795325112867385, 1.000000000000000000, 0.9238795325112867385, 1.000000000000000000, 0.9238795325112867385, 1.000000000000000000, 0.9238795325112867385, 1.000000000000000000, 0.9238795325112867385, 1.000000000000000000, 0.9238795325112867385, 1.000000000000000000, 0.9238795325112867385, 1.000000000000000000, 0.9238795325112867385, 1.000000000000000000, 0.9238795325112867385, 1.000000000000000000, 0.9238795325112867385, 1.000000000000000000, 0.9694574366903154772, 0.9634246591005992677),
 ( 1.000000000000000000, 0.9238795325112867385, 1.000000000000000000, 0.9238795325112867385, 1.000000000000000000, 0.9238795325112867385, 1.000000000000000000, 0.9238795325112867385, 1.000000000000000000, 0.9238795325112867385, 1.000000000000000000, 0.9238795325112867385, 1.000000000000000000, 0.9238795325112867385, 1.000000000000000000, 0.9238795325112867385, 1.000000000000000000, 0.9238795325112867385, 1.000000000000000000, 0.9238795325112867385, 1.000000000000000000, 0.9238795325112867385, 1.000000000000000000, 0.9238795325112867385, 1.000000000000000000, 0.9238795325112867385, 1.000000000000000000, 0.9238795325112867385, 1.000000000000000000, 0.9238795325112867385, 1.000000000000000000, 0.9238795325112867385, 1.000000000000000000, 0.9238795325112867385, 1.000000000000000000, 0.9238795325112867385, 1.000000000000000000, 0.9238795325112867385, 1.000000000000000000, 0.9238795325112867385, 1.000000000000000000, 0.9238795325112867385, 1.000000000000000000, 0.9238795325112867385, 1.000000000000000000, 0.9238795325112867385, 1.000000000000000000, 0.9238795325112867385, 1.000000000000000000, 0.9238795325112867385, 1.000000000000000000, 0.9238795325112867385, 1.000000000000000000, 0.9238795325112867385, 1.000000000000000000, 0.9238795325112867385, 1.000000000000000000, 0.9238795325112867385, 1.000000000000000000, 0.9238795325112867385, 1.000000000000000000, 0.9238795325112867385, 1.000000000000000000, 0.9238795325112867385, 1.000000000000000000, 0.9238795325112867385, 1.000000000000000000, 0.9238795325112867385, 1.000000000000000000, 0.9238795325112867385, 1.000000000000000000, 0.9238795325112867385, 1.000000000000000000, 0.9238795325112867385, 1.000000000000000000, 0.9238795325112867385, 1.000000000000000000, 0.9694574366903154772, 0.9634246591005992677) ) ) 
 REPRESENTATION_ITEM ( '' )  SURFACE ( )  );
#5302 = CARTESIAN_POINT ( 'NONE',  ( 8.312768060858603647, 41.62767341174088642, 77.52218233473911368 ) ) ;
#5303 = LINE ( 'NONE', #2134, #3491 ) ;
#5304 = ADVANCED_FACE ( 'NONE', ( #2069 ), #13042, .F. ) ;
#5305 = CARTESIAN_POINT ( 'NONE',  ( 5.869592478971509486, 51.15265838819242106, 78.02050120841747116 ) ) ;
#5306 = ORIENTED_EDGE ( 'NONE', *, *, #8625, .T. ) ;
#5307 = CARTESIAN_POINT ( 'NONE',  ( 8.382617512212860333, 42.28137902014101712, 79.47377622490290605 ) ) ;
#5308 = DIRECTION ( 'NONE',  ( 1.000000000000000000, 0.000000000000000000, 0.000000000000000000 ) ) ;
#5309 = DIRECTION ( 'NONE',  ( 3.893792155548169402E-16, 7.183611964723547524E-17, -1.000000000000000000 ) ) ;
#5310 = ORIENTED_EDGE ( 'NONE', *, *, #8034, .F. ) ;
#5311 = CARTESIAN_POINT ( 'NONE',  ( -3.567000345541168738, 47.45638922224109280, 95.05433879953099563 ) ) ;
#5312 = LINE ( 'NONE', #10244, #9880 ) ;
#5313 = CARTESIAN_POINT ( 'NONE',  ( -5.154188915835984375, 42.64120994080404614, 90.96121380123797451 ) ) ;
#5314 = ADVANCED_FACE ( 'NONE', ( #19724 ), #15053, .T. ) ;
#5315 = CARTESIAN_POINT ( 'NONE',  ( 1.828298387814866865, 52.94252695135357811, 76.99833242929096855 ) ) ;
#5316 = EDGE_CURVE ( 'NONE', #11104, #12307, #18138, .T. ) ;
#5317 = CARTESIAN_POINT ( 'NONE',  ( -5.784195910403845176, 44.99242805365518194, 94.63308880123798872 ) ) ;
#5318 = UNCERTAINTY_MEASURE_WITH_UNIT (LENGTH_MEASURE( 1.000000000000000082E-05 ), #2326, 'distance_accuracy_value', 'NONE');
#5319 = DIRECTION ( 'NONE',  ( -0.9485903129789527988, 0.3165065846431829311, -8.934458285744989980E-17 ) ) ;
#5320 = ORIENTED_EDGE ( 'NONE', *, *, #12393, .T. ) ;
#5321 = EDGE_CURVE ( 'NONE', #16316, #14474, #11863, .T. ) ;
#5322 = CARTESIAN_POINT ( 'NONE',  ( -2.627048034785010699, 48.88511640015991588, 92.45433879952862810 ) ) ;
#5323 = EDGE_CURVE ( 'NONE', #11825, #4581, #3755, .T. ) ;
#5324 = ORIENTED_EDGE ( 'NONE', *, *, #11596, .T. ) ;
#5325 = VECTOR ( 'NONE', #17943, 1000.000000000000000 ) ;
#5326 = DIRECTION ( 'NONE',  ( -0.9539696396349547358, 0.2999031954727300886, -9.315070279690498823E-17 ) ) ;
#5327 = B_SPLINE_CURVE_WITH_KNOTS ( 'NONE', 3,
 ( #2968, #14667, #1271, #7765, #12762, #3081, #14243, #15961, #1379, #9581, #17759, #20927, #6362, #14567, #12971 ),
 .UNSPECIFIED., .F., .F.,
 ( 4, 1, 1, 1, 1, 1, 1, 1, 1, 1, 1, 1, 4 ),
 ( 0.000000000000000000, 0.1159675137638946224, 0.2163545172648820292, 0.3041323377849299292, 0.3879046361115746633, 0.4329802283776429395, 0.4868190193916722697, 0.5485431915433492955, 0.6192726642024330985, 0.7001311270025748490, 0.7903233920492748199, 0.8897556754282296421, 1.000000000000000000 ),
 .UNSPECIFIED. ) ;
#5328 = CARTESIAN_POINT ( 'NONE',  ( -3.350035803220276609, 49.20851703305431357, 91.97683880123797451 ) ) ;
#5329 = EDGE_CURVE ( 'NONE', #7903, #19292, #6417, .T. ) ;
#5330 = ORIENTED_EDGE ( 'NONE', *, *, #18204, .F. ) ;
#5331 = CARTESIAN_POINT ( 'NONE',  ( 2.635245049009969254, 48.69372030666295359, 92.64183879611699979 ) ) ;
#5332 = CARTESIAN_POINT ( 'NONE',  ( -0.07555581626192474365, 50.25084051303456079, 69.06567965797609077 ) ) ;
#5333 = CARTESIAN_POINT ( 'NONE',  ( 0.5221537403065009686, 44.16218137147968292, 79.40903933791013003 ) ) ;
#5334 = FACE_OUTER_BOUND ( 'NONE', #13206, .T. ) ;
#5335 = ORIENTED_EDGE ( 'NONE', *, *, #5452, .T. ) ;
#5336 = CARTESIAN_POINT ( 'NONE',  ( -1.477846259693498920, 49.81903562097206617, 75.21119304902337888 ) ) ;
#5337 = AXIS2_PLACEMENT_3D ( 'NONE', #1905, #3286, #196 ) ;
#5338 = ORIENTED_EDGE ( 'NONE', *, *, #15993, .T. ) ;
#5339 = CARTESIAN_POINT ( 'NONE',  ( -3.034344139812558794, 48.41735725404262070, 95.05433879953095300 ) ) ;
#5340 = CARTESIAN_POINT ( 'NONE',  ( -6.990385563023369109, 41.19984844700349669, 76.84875211988632770 ) ) ;
#5341 = DIRECTION ( 'NONE',  ( 0.5670994908670431434, -0.8236492988270800453, -6.036271672687318437E-17 ) ) ;
#5342 = CARTESIAN_POINT ( 'NONE',  ( 7.864691922653266332, 47.81281597943210215, 78.56977997600147035 ) ) ;
#5343 = B_SPLINE_CURVE_WITH_KNOTS ( 'NONE', 3,
 ( #12304, #12088, #18786, #1011 ),
 .UNSPECIFIED., .F., .F.,
 ( 4, 4 ),
 ( 0.01428392225856168346, 0.01552286970674640783 ),
 .UNSPECIFIED. ) ;
#5344 = VECTOR ( 'NONE', #5443, 1000.000000000000000 ) ;
#5345 = CARTESIAN_POINT ( 'NONE',  ( -4.007890887056452023, 40.01116025973682611, 95.14183879782397923 ) ) ;
#5346 = CARTESIAN_POINT ( 'NONE',  ( 8.207311740369052089, 47.02196222218739763, 75.43669174070734584 ) ) ;
#5347 = ORIENTED_EDGE ( 'NONE', *, *, #3144, .T. ) ;
#5348 = EDGE_CURVE ( 'NONE', #19575, #17248, #18539, .T. ) ;
#5349 = CARTESIAN_POINT ( 'NONE',  ( -1.477846259693492925, 47.62628298661744708, 45.55433879953100273 ) ) ;
#5350 = DIRECTION ( 'NONE',  ( 1.000000000000000000, 1.213411507412056509E-16, 0.000000000000000000 ) ) ;
#5351 = AXIS2_PLACEMENT_3D ( 'NONE', #4041, #12047, #8849 ) ;
#5352 = ORIENTED_EDGE ( 'NONE', *, *, #534, .T. ) ;
#5353 = CARTESIAN_POINT ( 'NONE',  ( -1.293305036878872993, 38.38734275159215059, 75.45433879953087342 ) ) ;
#5354 = CARTESIAN_POINT ( 'NONE',  ( -2.077846259693550746, 39.65884927180063357, 95.41433879953098085 ) ) ;
#5355 = CARTESIAN_POINT ( 'NONE',  ( -5.058133621542618030, 44.89684013992257405, 92.67996379953099506 ) ) ;
#5356 = ORIENTED_EDGE ( 'NONE', *, *, #5624, .T. ) ;
#5357 = DIRECTION ( 'NONE',  ( 1.000000000000000000, -0.000000000000000000, -0.000000000000000000 ) ) ;
#5358 = CARTESIAN_POINT ( 'NONE',  ( -5.419656513257916863, 37.61074265007806616, 75.48149882193594351 ) ) ;
#5359 = ORIENTED_EDGE ( 'NONE', *, *, #7426, .F. ) ;
#5360 = CARTESIAN_POINT ( 'NONE',  ( -2.754305542028548714, 39.77410375191711722, 95.05433879953098142 ) ) ;
#5361 = LINE ( 'NONE', #8260, #12892 ) ;
#5362 = ORIENTED_EDGE ( 'NONE', *, *, #12093, .T. ) ;
#5363 = CARTESIAN_POINT ( 'NONE',  ( -4.917446439638612610, 37.23978029895120301, 77.90454030471208569 ) ) ;
#5364 = CARTESIAN_POINT ( 'NONE',  ( 4.394343283833276992, 39.11584570990505938, 94.00808880123797451 ) ) ;
#5365 = ORIENTED_EDGE ( 'NONE', *, *, #5878, .T. ) ;
#5366 = CARTESIAN_POINT ( 'NONE',  ( -4.346214470222207638, 50.75228047588369407, 75.98997946140892168 ) ) ;
#5367 = LINE ( 'NONE', #18360, #4417 ) ;
#5368 = CARTESIAN_POINT ( 'NONE',  ( 5.146043734657006041, 40.41782908280415398, 90.15009084312077903 ) ) ;
#5369 = VECTOR ( 'NONE', #15364, 1000.000000000000000 ) ;
#5370 =( LENGTH_UNIT ( ) NAMED_UNIT ( * ) SI_UNIT ( .MILLI., .METRE. ) );
#5371 = CARTESIAN_POINT ( 'NONE',  ( 10.77494014480653917, 42.96218137147968008, 61.80715055817104542 ) ) ;
#5372 = CARTESIAN_POINT ( 'NONE',  ( -1.293305036878872549, 38.38734275159215059, 72.45432679953087529 ) ) ;
#5373 = ORIENTED_EDGE ( 'NONE', *, *, #8944, .F. ) ;
#5374 = ORIENTED_EDGE ( 'NONE', *, *, #19385, .T. ) ;
#5375 = CARTESIAN_POINT ( 'NONE',  ( 5.201216021426783520, 36.68989574863261538, 75.41205140984322952 ) ) ;
#5376 = VERTEX_POINT ( 'NONE', #2176 ) ;
#5377 = PLANE ( 'NONE',  #8486 ) ;
#5378 = CARTESIAN_POINT ( 'NONE',  ( 0.5264430316339508975, 52.35469197387742923, 77.38663191694250543 ) ) ;
#5379 = DIRECTION ( 'NONE',  ( 1.402518428993831183E-16, -1.000000000000000000, 3.469446951953617640E-16 ) ) ;
#5380 = EDGE_LOOP ( 'NONE', ( #16768, #16972, #15957, #14788 ) ) ;
#5381 = AXIS2_PLACEMENT_3D ( 'NONE', #18107, #1928, #8425 ) ;
#5382 = CARTESIAN_POINT ( 'NONE',  ( -3.944959226007136888, 38.51060946023304865, 76.38448585835440952 ) ) ;
#5383 = VERTEX_POINT ( 'NONE', #5896 ) ;
#5384 = DIRECTION ( 'NONE',  ( 1.110223024625156540E-16, 1.000000000000000000, 5.922860397471808077E-17 ) ) ;
#5385 = ADVANCED_FACE ( 'NONE', ( #15263, #5788 ), #10804, .F. ) ;
#5386 = CARTESIAN_POINT ( 'NONE',  ( 0.0004206109058209459473, 52.21206128023939641, 75.41772606587693417 ) ) ;
#5387 = CARTESIAN_POINT ( 'NONE',  ( 8.596205818237969254, 40.55709867257476731, 75.50010622114506020 ) ) ;
#5388 = CARTESIAN_POINT ( 'NONE',  ( 2.916646314870772194, 38.79555996194921619, 92.55433879953098142 ) ) ;
#5389 = LINE ( 'NONE', #16691, #12155 ) ;
#5390 = CARTESIAN_POINT ( 'NONE',  ( -0.3407952795220794417, 52.92038597201553074, 75.53001665154320676 ) ) ;
#5391 = CARTESIAN_POINT ( 'NONE',  ( -2.416137431568557314, 39.07291177436112406, 95.02371380123797451 ) ) ;
#5392 = CARTESIAN_POINT ( 'NONE',  ( -4.361665858399769391, 37.57520132541210245, 75.97198585835440099 ) ) ;
#5393 = LINE ( 'NONE', #20077, #11219 ) ;
#5394 = CARTESIAN_POINT ( 'NONE',  ( 0.5221537403065015237, 44.16218137147968292, 75.45433879953088763 ) ) ;
#5395 = CARTESIAN_POINT ( 'NONE',  ( -5.058133621542618030, 44.89684013992257405, 95.49246380294496817 ) ) ;
#5396 = VECTOR ( 'NONE', #15725, 1000.000000000000000 ) ;
#5397 = CARTESIAN_POINT ( 'NONE',  ( 0.5221537403065105165, 44.16218137147969713, 50.55433879953100273 ) ) ;
#5398 = CARTESIAN_POINT ( 'NONE',  ( 0.3332418091178914743, 52.96755426434335590, 76.35041178738960355 ) ) ;
#5399 = CIRCLE ( 'NONE', #17319, 8.199999999999995737 ) ;
#5400 = ORIENTED_EDGE ( 'NONE', *, *, #20510, .F. ) ;
#5401 = CARTESIAN_POINT ( 'NONE',  ( 32.72215374030650281, 44.16218137147968292, 45.55433879953098852 ) ) ;
#5402 = DIRECTION ( 'NONE',  ( 1.000000000000000000, 0.000000000000000000, 0.000000000000000000 ) ) ;
#5403 = CARTESIAN_POINT ( 'NONE',  ( -4.529140103682425256, 37.70758999251661692, 78.69750623079058016 ) ) ;
#5404 = CARTESIAN_POINT ( 'NONE',  ( -2.416137431568557314, 39.07291177436112406, 92.52371380123797451 ) ) ;
#5405 = VECTOR ( 'NONE', #16444, 1000.000000000000000 ) ;
#5406 = CARTESIAN_POINT ( 'NONE',  ( 0.5221537403065020788, 52.36218137147968577, 83.03825919817350609 ) ) ;
#5407 = DIRECTION ( 'NONE',  ( -0.3165065846431827090, -0.9485903129789529098, -2.188653791613874994E-16 ) ) ;
#5408 = ADVANCED_FACE ( 'NONE', ( #15580 ), #11251, .T. ) ;
#5409 = CARTESIAN_POINT ( 'NONE',  ( -1.477846259693495146, 49.81903562097207327, 85.15433879953098995 ) ) ;
#5410 = VERTEX_POINT ( 'NONE', #20238 ) ;
#5411 = EDGE_LOOP ( 'NONE', ( #7846, #16578, #2226, #1934 ) ) ;
#5412 = TOROIDAL_SURFACE ( 'NONE', #9198, 13.99999999999999645, 4.000000000000000000 ) ;
#5413 = CARTESIAN_POINT ( 'NONE',  ( 9.122633311574107395, 42.13483526604063201, 79.44701590970058191 ) ) ;
#5414 = DIRECTION ( 'NONE',  ( 3.893792155548169402E-16, 7.183611964723547524E-17, -1.000000000000000000 ) ) ;
#5415 = CARTESIAN_POINT ( 'NONE',  ( -4.197504116382902772, 37.45658124447859905, 78.86215563453255584 ) ) ;
#5416 = VERTEX_POINT ( 'NONE', #5670 ) ;
#5417 = DIRECTION ( 'NONE',  ( 0.9534635866061452747, 0.3015081906286223301, 5.201162577080931668E-16 ) ) ;
#5418 = CARTESIAN_POINT ( 'NONE',  ( 9.353817388681445522, 42.82770861117572281, 78.41904468188381827 ) ) ;
#5419 = VECTOR ( 'NONE', #15908, 1000.000000000000000 ) ;
#5420 = DIRECTION ( 'NONE',  ( -2.909222284125554245E-16, -0.7071067811865460184, 0.7071067811865490160 ) ) ;
#5421 = CARTESIAN_POINT ( 'NONE',  ( 4.987494971863720927, 47.58855820898865829, 90.02371380294498238 ) ) ;
#5422 = B_SPLINE_CURVE_WITH_KNOTS ( 'NONE', 3,
 ( #9163, #12044, #2346, #4243, #20528, #5954, #15655, #12251, #7340, #13943, #10562, #2459, #1071, #5741, #10770 ),
 .UNSPECIFIED., .F., .F.,
 ( 4, 1, 1, 1, 1, 1, 1, 1, 1, 1, 1, 1, 4 ),
 ( 0.000000000000000000, 0.1112587825215290704, 0.2075697215801151074, 0.2973595701983123840, 0.3838682041569268510, 0.4304545292676484891, 0.4853887544929457731, 0.5479167518276804039, 0.6204346596782769341, 0.7008860551074163059, 0.7907659637769564043, 0.8904818903857688595, 1.000000000000000000 ),
 .UNSPECIFIED. ) ;
#5423 = CARTESIAN_POINT ( 'NONE',  ( -7.232524501155468855, 41.51784650842750324, 78.89406302991613984 ) ) ;
#5424 = CARTESIAN_POINT ( 'NONE',  ( -3.131747484992676078, 36.83477141872401006, 78.11242031084098869 ) ) ;
#5425 = EDGE_CURVE ( 'NONE', #10288, #18561, #18873, .T. ) ;
#5426 = CARTESIAN_POINT ( 'NONE',  ( -4.524181921268124462, 40.28999182795290324, 96.03933880123798872 ) ) ;
#5427 = AXIS2_PLACEMENT_3D ( 'NONE', #2294, #808, #13682 ) ;
#5428 = VECTOR ( 'NONE', #14496, 1000.000000000000227 ) ;
#5429 = CARTESIAN_POINT ( 'NONE',  ( -8.146098697889676998, 42.64342655637305768, 79.20824032290880723 ) ) ;
#5430 = VERTEX_POINT ( 'NONE', #20178 ) ;
#5431 = LINE ( 'NONE', #13525, #3445 ) ;
#5432 = ORIENTED_EDGE ( 'NONE', *, *, #10732, .F. ) ;
#5433 = VECTOR ( 'NONE', #3872, 1000.000000000000000 ) ;
#5434 = CARTESIAN_POINT ( 'NONE',  ( 2.392664886727894125, 47.70104341108812918, 77.28382765310962554 ) ) ;
#5435 = EDGE_CURVE ( 'NONE', #14176, #16316, #20698, .T. ) ;
#5436 = CARTESIAN_POINT ( 'NONE',  ( -0.9988176903691428077, 49.83852402762217082, 90.64871380123798872 ) ) ;
#5437 = ORIENTED_EDGE ( 'NONE', *, *, #6256, .F. ) ;
#5438 = EDGE_CURVE ( 'NONE', #19018, #983, #2899, .T. ) ;
#5439 = LINE ( 'NONE', #11954, #2829 ) ;
#5440 = ADVANCED_FACE ( 'NONE', ( #10425 ), #1150, .T. ) ;
#5441 = CARTESIAN_POINT ( 'NONE',  ( 2.522153740306493308, 49.81903562097208749, 59.21119304902340019 ) ) ;
#5442 = CARTESIAN_POINT ( 'NONE',  ( -3.553498346352079285, 52.06564182703182553, 79.13154374754441278 ) ) ;
#5443 = DIRECTION ( 'NONE',  ( 1.540237394707284220E-16, 1.793354297423764243E-16, -1.000000000000000000 ) ) ;
#5444 = CARTESIAN_POINT ( 'NONE',  ( -0.9388773962491537839, 52.84004908296358138, 77.77566232894263010 ) ) ;
#5445 = CARTESIAN_POINT ( 'NONE',  ( 0.5623910665089989491, 52.35440851336043977, 78.93584868477675798 ) ) ;
#5446 = ORIENTED_EDGE ( 'NONE', *, *, #7159, .T. ) ;
#5447 = AXIS2_PLACEMENT_3D ( 'NONE', #7070, #14756, #16563 ) ;
#5448 = CARTESIAN_POINT ( 'NONE',  ( 5.748274343403733333, 51.24227120794373747, 77.94845644658968808 ) ) ;
#5449 = ORIENTED_EDGE ( 'NONE', *, *, #11800, .F. ) ;
#5450 = CARTESIAN_POINT ( 'NONE',  ( 2.035123479059381957, 36.10296785094195826, 76.16022115247204738 ) ) ;
#5451 = CARTESIAN_POINT ( 'NONE',  ( 0.5221537403065064087, 48.16218137147969003, 66.55433879953099563 ) ) ;
#5452 = EDGE_CURVE ( 'NONE', #7102, #18032, #8480, .T. ) ;
#5453 = CARTESIAN_POINT ( 'NONE',  ( 0.5221537403065013017, 44.16218137147968292, 77.05433879953086773 ) ) ;
#5454 = CARTESIAN_POINT ( 'NONE',  ( -7.292942379224079730, 40.11689118711894508, 78.38760373728354125 ) ) ;
#5455 = FACE_OUTER_BOUND ( 'NONE', #1002, .T. ) ;
#5456 = CARTESIAN_POINT ( 'NONE',  ( 5.176818351154000020, 40.65164613849449182, 95.49246367200940711 ) ) ;
#5457 = CARTESIAN_POINT ( 'NONE',  ( 5.489796880388170486, 37.64302049704706121, 76.21413800766271152 ) ) ;
#5458 = CARTESIAN_POINT ( 'NONE',  ( -4.561334846378493069, 51.34547876336230843, 75.36123162944792853 ) ) ;
#5459 = ORIENTED_EDGE ( 'NONE', *, *, #5040, .F. ) ;
#5460 = CARTESIAN_POINT ( 'NONE',  ( 8.792941515635112282, 41.14672803835393466, 78.80099766627323277 ) ) ;
#5461 = PRODUCT_DEFINITION_FORMATION_WITH_SPECIFIED_SOURCE ( 'ANY', '', #18386, .NOT_KNOWN. ) ;
#5462 = ORIENTED_EDGE ( 'NONE', *, *, #19872, .F. ) ;
#5463 = DIRECTION ( 'NONE',  ( 0.8043570849675437673, -0.5941461771841298756, 1.733862608136950550E-17 ) ) ;
#5464 = CARTESIAN_POINT ( 'NONE',  ( 1.256812508749381774, 49.74246873332880625, 92.36746379953098085 ) ) ;
#5465 = CARTESIAN_POINT ( 'NONE',  ( -0.2125050281363792815, 38.58189400963055959, 91.74246379953099506 ) ) ;
#5466 = PRODUCT_DEFINITION_SHAPE ( 'NONE', 'NONE',  #21037 ) ;
#5467 = ORIENTED_EDGE ( 'NONE', *, *, #9631, .T. ) ;
#5468 = SURFACE_STYLE_FILL_AREA ( #8682 ) ;
#5469 = DIRECTION ( 'NONE',  ( -1.540237394707284220E-16, -1.793354297423764243E-16, 1.000000000000000000 ) ) ;
#5470 = CARTESIAN_POINT ( 'NONE',  ( 11.32022995165976198, 36.96218137147968719, 93.55433879953098142 ) ) ;
#5471 = CARTESIAN_POINT ( 'NONE',  ( -4.785381074711875016, 51.18538353145122954, 78.79723525346945223 ) ) ;
#5472 = EDGE_CURVE ( 'NONE', #867, #6210, #1043, .T. ) ;
#5473 = CARTESIAN_POINT ( 'NONE',  ( -0.8237052942265477018, 49.18499566818285018, 92.44558879953099506 ) ) ;
#5474 = VERTEX_POINT ( 'NONE', #14017 ) ;
#5475 = CARTESIAN_POINT ( 'NONE',  ( 2.103244830950438349, 52.20830968050383802, 78.56392946132328348 ) ) ;
#5476 = CARTESIAN_POINT ( 'NONE',  ( 5.025485839985549319, 41.56218137147963887, 90.72683879953099506 ) ) ;
#5477 = AXIS2_PLACEMENT_3D ( 'NONE', #3585, #19752, #17853 ) ;
#5478 = VERTEX_POINT ( 'NONE', #17208 ) ;
#5479 = CARTESIAN_POINT ( 'NONE',  ( -4.592862224480082745, 51.32295045326189609, 75.97198585835440099 ) ) ;
#5480 = LINE ( 'NONE', #12412, #3064 ) ;
#5481 = ADVANCED_FACE ( 'NONE', ( #5932 ), #18491, .T. ) ;
#5482 = VECTOR ( 'NONE', #2042, 1000.000000000000000 ) ;
#5483 = CARTESIAN_POINT ( 'NONE',  ( -3.350035803220276609, 49.20851703305431357, 90.72683880123797451 ) ) ;
#5484 = EDGE_CURVE ( 'NONE', #8638, #16327, #12112, .T. ) ;
#5485 = APPLICATION_PROTOCOL_DEFINITION ( 'draft international standard', 'automotive_design', 1998, #435 ) ;
#5486 = CARTESIAN_POINT ( 'NONE',  ( -4.534948301111437985, 37.71188027398896736, 76.38448585835440952 ) ) ;
#5487 = CARTESIAN_POINT ( 'NONE',  ( 0.5221537403065020788, 52.36218137147968577, 48.36106904222365444 ) ) ;
#5488 = CARTESIAN_POINT ( 'NONE',  ( -3.100601612254845207, 36.80584749508156506, 78.55896582016906393 ) ) ;
#5489 = B_SPLINE_CURVE_WITH_KNOTS ( 'NONE', 3,
 ( #7573, #2783, #760, #18633, #2470, #5964, #15774, #12462, #7245, #5189, #19966 ),
 .UNSPECIFIED., .F., .F.,
 ( 4, 1, 1, 1, 1, 1, 1, 1, 4 ),
 ( 0.000000000000000000, 0.1116983415361904319, 0.2084596166200352318, 0.2965296202300037876, 0.3842340601578678183, 0.4893760538913073388, 0.6260801343201788383, 0.7954079187270842732, 1.000000000000000000 ),
 .UNSPECIFIED. ) ;
#5490 = ORIENTED_EDGE ( 'NONE', *, *, #2497, .F. ) ;
#5491 = ORIENTED_EDGE ( 'NONE', *, *, #11737, .T. ) ;
#5492 = DIRECTION ( 'NONE',  ( 1.540237394707284220E-16, 1.793354297423764243E-16, -1.000000000000000000 ) ) ;
#5493 = EDGE_LOOP ( 'NONE', ( #18846, #18145, #8443, #1222, #4319, #18397 ) ) ;
#5494 = VECTOR ( 'NONE', #19305, 1000.000000000000000 ) ;
#5495 = B_SPLINE_CURVE_WITH_KNOTS ( 'NONE', 3,
 ( #9532, #1539, #9839, #16015, #1644, #3235, #16328, #1436, #19504, #7922, #14510, #20978, #14409, #6309, #9737, #8126, #13029, #4918, #11439, #5339, #457, #16744, #3646, #6837, #3857 ),
 .UNSPECIFIED., .F., .F.,
 ( 4, 2, 2, 2, 2, 2, 2, 2, 2, 1, 2, 2, 4 ),
 ( 1.624908565367659545E-10, 0.001304848329475893996, 0.001957272412968412423, 0.002609696496460930416, 0.003914544663445968138, 0.004566968746938486999, 0.005219392830431005860, 0.006524240997416045316, 0.007176665080908565045, 0.007829089164401083906, 0.008481513247893604501, 0.009133937331386125097, 0.01043878549837116282 ),
 .UNSPECIFIED. ) ;
#5496 = CARTESIAN_POINT ( 'NONE',  ( -5.086207797142201947, 38.17983230318012744, 75.51021574373382350 ) ) ;
#5497 = LINE ( 'NONE', #17202, #5835 ) ;
#5498 = CARTESIAN_POINT ( 'NONE',  ( 10.77494014480653561, 42.96218137147968008, 77.40433879953098995 ) ) ;
#5499 = VECTOR ( 'NONE', #18826, 1000.000000000000000 ) ;
#5500 = EDGE_LOOP ( 'NONE', ( #15221, #12806 ) ) ;
#5501 = VERTEX_POINT ( 'NONE', #15305 ) ;
#5502 = LINE ( 'NONE', #16889, #9986 ) ;
#5503 = ORIENTED_EDGE ( 'NONE', *, *, #11326, .F. ) ;
#5504 = CARTESIAN_POINT ( 'NONE',  ( -3.798187483714128287, 36.41302879471073339, 77.61986069475027250 ) ) ;
#5505 = DIRECTION ( 'NONE',  ( 3.154042683594179442E-15, -3.469446951953613203E-16, -1.000000000000000000 ) ) ;
#5506 = DIRECTION ( 'NONE',  ( 1.402518428993831183E-16, -1.000000000000000000, 3.469446951953617640E-16 ) ) ;
#5507 = CARTESIAN_POINT ( 'NONE',  ( 4.187809154542623702, 51.47009103659679852, 77.37197156638603701 ) ) ;
#5508 = FACE_OUTER_BOUND ( 'NONE', #20974, .T. ) ;
#5509 = ADVANCED_FACE ( 'NONE', ( #7415 ), #9134, .T. ) ;
#5510 = DIRECTION ( 'NONE',  ( -0.5941461771851691553, -0.8043570849667760481, -2.357623395011396791E-16 ) ) ;
#5511 = CARTESIAN_POINT ( 'NONE',  ( 0.8455664304067509462, 52.35217556859831944, 77.76169174070734869 ) ) ;
#5513 = DIRECTION ( 'NONE',  ( 3.154042683594179442E-15, 0.000000000000000000, -1.000000000000000000 ) ) ;
#5512 = VECTOR ( 'NONE', #9718, 1000.000000000000000 ) ;
#5514 = FACE_OUTER_BOUND ( 'NONE', #19168, .T. ) ;
#5515 = CARTESIAN_POINT ( 'NONE',  ( -3.943187491250720544, 40.73580453397070755, 93.14871380294496817 ) ) ;
#5516 = CIRCLE ( 'NONE', #20461, 4.200000000000000178 ) ;
#5517 = CARTESIAN_POINT ( 'NONE',  ( -5.769203958596529347, 48.43638519259695840, 75.45433879953087342 ) ) ;
#5518 = VERTEX_POINT ( 'NONE', #2741 ) ;
#5519 = CARTESIAN_POINT ( 'NONE',  ( 0.3281079151674232142, 52.35625600837144589, 76.41414202728766725 ) ) ;
#5520 = ORIENTED_EDGE ( 'NONE', *, *, #14981, .T. ) ;
#5521 = LINE ( 'NONE', #3919, #313 ) ;
#5522 = DIRECTION ( 'NONE',  ( -4.731737692062861008E-17, 0.7071067811865475727, 0.7071067811865475727 ) ) ;
#5523 = CARTESIAN_POINT ( 'NONE',  ( -3.653812822066824673, 51.99396077543343608, 79.24282704039583791 ) ) ;
#5524 = CARTESIAN_POINT ( 'NONE',  ( -5.154188915835984375, 42.64120994080404614, 93.61746380123797451 ) ) ;
#5525 = AXIS2_PLACEMENT_3D ( 'NONE', #12495, #10918, #3125 ) ;
#5526 = CARTESIAN_POINT ( 'NONE',  ( -4.887610060180215932, 37.21774136732800997, 76.16751655709613544 ) ) ;
#5527 = DIRECTION ( 'NONE',  ( 1.000000000000000000, 0.000000000000000000, 0.000000000000000000 ) ) ;
#5528 = CARTESIAN_POINT ( 'NONE',  ( 5.611423337425062385, 41.22389019960463230, 91.58621380123798872 ) ) ;
#5529 = EDGE_CURVE ( 'NONE', #10926, #19585, #2633, .T. ) ;
#5530 = CIRCLE ( 'NONE', #1807, 8.199999999999995737 ) ;
#5531 = CARTESIAN_POINT ( 'NONE',  ( 3.983393151002396326, 36.72848634532711287, 75.45433879953088763 ) ) ;
#5532 = ORIENTED_EDGE ( 'NONE', *, *, #20293, .T. ) ;
#5533 = CARTESIAN_POINT ( 'NONE',  ( 9.223886884231923489, 42.43829864670298946, 79.29919401074631935 ) ) ;
#5534 = CARTESIAN_POINT ( 'NONE',  ( 27.63948732994508006, 45.16218137147969003, 76.90433879953101837 ) ) ;
#5535 = CARTESIAN_POINT ( 'NONE',  ( -4.159936764691080313, 37.43031352553058611, 78.66301351013966325 ) ) ;
#5536 = ORIENTED_EDGE ( 'NONE', *, *, #9033, .F. ) ;
#5537 = DIRECTION ( 'NONE',  ( -1.000000000000000000, -3.942553354492745503E-16, 0.000000000000000000 ) ) ;
#5538 = CARTESIAN_POINT ( 'NONE',  ( 5.739698376139652503, 51.24860592950068394, 77.28905211432859801 ) ) ;
#5539 = CARTESIAN_POINT ( 'NONE',  ( -8.191524702974342986, 42.93261893028977738, 75.65823721589713102 ) ) ;
#5540 = CARTESIAN_POINT ( 'NONE',  ( 8.722153740306483272, 51.36218137147968577, 95.05433879953098142 ) ) ;
#5541 = CARTESIAN_POINT ( 'NONE',  ( -7.285980590069234708, 41.68689144931414603, 78.93669174070734584 ) ) ;
#5542 = VECTOR ( 'NONE', #19953, 1000.000000000000000 ) ;
#5543 = CARTESIAN_POINT ( 'NONE',  ( -7.088924111666181638, 47.02415304900689108, 77.58227997600145898 ) ) ;
#5544 = CARTESIAN_POINT ( 'NONE',  ( -5.154188915835984375, 42.64120994080404614, 93.46121380123797451 ) ) ;
#5545 = EDGE_CURVE ( 'NONE', #14408, #20491, #720, .T. ) ;
#5546 = CARTESIAN_POINT ( 'NONE',  ( -8.192078482032012943, 42.93655631659661509, 78.28007409364852265 ) ) ;
#5547 = VERTEX_POINT ( 'NONE', #9028 ) ;
#5548 = CARTESIAN_POINT ( 'NONE',  ( 1.720761564499668772, 52.27449377805036335, 75.61803672508528962 ) ) ;
#5549 = EDGE_LOOP ( 'NONE', ( #1240, #3354, #13584, #9503 ) ) ;
#5550 = LINE ( 'NONE', #2254, #11582 ) ;
#5551 = CARTESIAN_POINT ( 'NONE',  ( 5.146041124512939824, 40.41782456190201600, 90.15009067557426192 ) ) ;
#5552 = ORIENTED_EDGE ( 'NONE', *, *, #8407, .F. ) ;
#5553 = CARTESIAN_POINT ( 'NONE',  ( 2.916646314870772194, 38.79555996194921619, 92.55433879953098142 ) ) ;
#5554 = VECTOR ( 'NONE', #6113, 1000.000000000000000 ) ;
#5555 = DIRECTION ( 'NONE',  ( -0.3165065846431824870, -0.9485903129789529098, 0.000000000000000000 ) ) ;
#5556 = EDGE_CURVE ( 'NONE', #14081, #8173, #20070, .T. ) ;
#5557 = CARTESIAN_POINT ( 'NONE',  ( -1.677846259693499542, 50.36218137147968577, 37.95170767603170248 ) ) ;
#5558 = CARTESIAN_POINT ( 'NONE',  ( 0.8487652345708711632, 52.95611971486915337, 77.67431885501342492 ) ) ;
#5559 = CARTESIAN_POINT ( 'NONE',  ( 5.583914945631950566, 51.36367687427735973, 77.16202479023476712 ) ) ;
#5560 = CARTESIAN_POINT ( 'NONE',  ( 0.4665392529312449854, 52.35516434013662490, 78.91893668031715947 ) ) ;
#5561 = ORIENTED_EDGE ( 'NONE', *, *, #3507, .F. ) ;
#5562 = CARTESIAN_POINT ( 'NONE',  ( 8.215015453637320775, 41.32318875976580586, 77.19119496967930161 ) ) ;
#5563 = ORIENTED_EDGE ( 'NONE', *, *, #426, .T. ) ;
#5564 = CARTESIAN_POINT ( 'NONE',  ( 5.665287683258889651, 37.02150436742986273, 75.36022115247205022 ) ) ;
#5565 = LINE ( 'NONE', #12067, #10459 ) ;
#5566 = CARTESIAN_POINT ( 'NONE',  ( 6.888069329080921399, 50.40035056576664374, 77.33077842133744184 ) ) ;
#5567 = CARTESIAN_POINT ( 'NONE',  ( 5.490991456512046121, 37.63909523311460248, 76.17446293557725312 ) ) ;
#5568 = CARTESIAN_POINT ( 'NONE',  ( -4.622577041588896485, 46.56120873422322859, 92.56371379782397923 ) ) ;
#5569 = CARTESIAN_POINT ( 'NONE',  ( -5.888951387225212386, 37.95739186912707908, 75.98496980016291502 ) ) ;
#5570 = ORIENTED_EDGE ( 'NONE', *, *, #7104, .F. ) ;
#5571 = CARTESIAN_POINT ( 'NONE',  ( 8.212727718596601889, 41.32804861490897252, 78.71078388337100762 ) ) ;
#5572 = EDGE_LOOP ( 'NONE', ( #11049, #8969, #3880, #16459 ) ) ;
#5573 = CARTESIAN_POINT ( 'NONE',  ( -3.795408181706389605, 50.97300633329361830, 75.39163409230444302 ) ) ;
#5574 = CARTESIAN_POINT ( 'NONE',  ( 5.544968037009670780, 45.50804040601273925, 94.63308879953099506 ) ) ;
#5575 = CARTESIAN_POINT ( 'NONE',  ( 3.948530577815480225, 39.69684013992245752, 91.89871379953099506 ) ) ;
#5576 = ORIENTED_EDGE ( 'NONE', *, *, #1069, .T. ) ;
#5577 = CARTESIAN_POINT ( 'NONE',  ( 6.828503391016846891, 43.33193468930419101, 94.16433880123797451 ) ) ;
#5578 = CARTESIAN_POINT ( 'NONE',  ( -4.524181921268124462, 40.28999182795290324, 94.78933880123805977 ) ) ;
#5579 = ORIENTED_EDGE ( 'NONE', *, *, #12878, .T. ) ;
#5580 = DIRECTION ( 'NONE',  ( -0.5670994908670485835, 0.8236492988270761595, 6.036271672687166828E-17 ) ) ;
#5581 = LINE ( 'NONE', #15490, #2374 ) ;
#5582 = VERTEX_POINT ( 'NONE', #8924 ) ;
#5583 = LINE ( 'NONE', #16970, #20713 ) ;
#5584 = CARTESIAN_POINT ( 'NONE',  ( -4.524181921268124462, 40.28999182795290324, 94.94558880123797451 ) ) ;
#5585 = ORIENTED_EDGE ( 'NONE', *, *, #16049, .F. ) ;
#5586 = CARTESIAN_POINT ( 'NONE',  ( 2.436687528221645582, 49.84925249003584469, 61.23980501161587853 ) ) ;
#5587 = CARTESIAN_POINT ( 'NONE',  ( 5.162414546052650266, 37.40137004776163820, 76.01747768713747178 ) ) ;
#5588 = APPLICATION_CONTEXT ( 'automotive_design' ) ;
#5589 = DIRECTION ( 'NONE',  ( 1.000000000000000000, 0.000000000000000000, -0.000000000000000000 ) ) ;
#5590 = APPLICATION_PROTOCOL_DEFINITION ( 'draft international standard', 'automotive_design', 1998, #11728 ) ;
#5592 = EDGE_CURVE ( 'NONE', #8992, #2511, #12328, .T. ) ;
#5591 = CARTESIAN_POINT ( 'NONE',  ( 0.3792072784172939581, 52.96103218509968968, 78.83587726364804382 ) ) ;
#5593 = FACE_OUTER_BOUND ( 'NONE', #17495, .T. ) ;
#5594 = ORIENTED_EDGE ( 'NONE', *, *, #755, .F. ) ;
#5595 = ADVANCED_FACE ( 'NONE', ( #9245 ), #13590, .F. ) ;
#5596 = ORIENTED_EDGE ( 'NONE', *, *, #12621, .T. ) ;
#5597 = CARTESIAN_POINT ( 'NONE',  ( 1.080293470566400904, 52.20967668552454910, 75.39315892328370694 ) ) ;
#5598 = ORIENTED_EDGE ( 'NONE', *, *, #7248, .T. ) ;
#5599 = CARTESIAN_POINT ( 'NONE',  ( -0.1859286156583806748, 52.33238584150070238, 79.44675239646682030 ) ) ;
#5600 = ADVANCED_FACE ( 'NONE', ( #18593 ), #18809, .F. ) ;
#5601 = CARTESIAN_POINT ( 'NONE',  ( 0.3294087859111602401, 52.35624566131623681, 77.66452874556115660 ) ) ;
#5602 = CARTESIAN_POINT ( 'NONE',  ( -5.154188915835984375, 42.64120994080404614, 96.11746380123797451 ) ) ;
#5603 = EDGE_LOOP ( 'NONE', ( #12942, #7052, #13651, #12822 ) ) ;
#5604 = ORIENTED_EDGE ( 'NONE', *, *, #5624, .F. ) ;
#5605 = CARTESIAN_POINT ( 'NONE',  ( 6.701747691083868474, 50.53797885426168079, 79.21482656134288902 ) ) ;
#5606 = VERTEX_POINT ( 'NONE', #17109 ) ;
#5607 = CARTESIAN_POINT ( 'NONE',  ( -3.847049756032938639, 36.44912138698024506, 77.64672866243046201 ) ) ;
#5608 = CARTESIAN_POINT ( 'NONE',  ( 24.43948732994508788, 36.35905713404684292, 74.70433879953100131 ) ) ;
#5609 = CARTESIAN_POINT ( 'NONE',  ( 7.814414200452987735, 40.59520435765989532, 75.60774188071792423 ) ) ;
#5610 = CARTESIAN_POINT ( 'NONE',  ( 11.22215374030650281, 42.96218137147968008, 69.80574467885101342 ) ) ;
#5611 = CARTESIAN_POINT ( 'NONE',  ( 4.584522445964598347, 52.10188785579612158, 77.22170381446332499 ) ) ;
#5612 = DIRECTION ( 'NONE',  ( -1.000000000000000000, -4.924280921909906060E-16, -5.626130192357177659E-16 ) ) ;
#5613 = CARTESIAN_POINT ( 'NONE',  ( 6.828503391016846891, 43.33193468930419101, 94.16433880123797451 ) ) ;
#5614 = CARTESIAN_POINT ( 'NONE',  ( 0.8412106418144055242, 52.35220991559214809, 77.64755553332491900 ) ) ;
#5615 = LINE ( 'NONE', #10106, #1359 ) ;
#5616 = DIRECTION ( 'NONE',  ( -5.595882180570345180E-16, 1.000000000000000000, 0.000000000000000000 ) ) ;
#5617 = CARTESIAN_POINT ( 'NONE',  ( -3.981178359372548492, 46.76218137147973408, 94.16433880294496817 ) ) ;
#5618 = CARTESIAN_POINT ( 'NONE',  ( 2.246318977524931704, 38.35943151540528362, 75.45433879953087342 ) ) ;
#5619 = CARTESIAN_POINT ( 'NONE',  ( 8.373444093038859393, 41.80954323823455354, 78.74360054667872078 ) ) ;
#5620 =( BOUNDED_CURVE ( )  B_SPLINE_CURVE ( 3, ( #19703, #5123, #7466, #13962 ),
 .UNSPECIFIED., .F., .F. ) 
 B_SPLINE_CURVE_WITH_KNOTS ( ( 4, 4 ),
 ( 1.230959417340772521, 1.276280841686757705 ),
 .UNSPECIFIED. ) 
 CURVE ( )  GEOMETRIC_REPRESENTATION_ITEM ( )  RATIONAL_B_SPLINE_CURVE ( ( 1.000000000000000000, 0.9998288380325438540, 0.9998288380325438540, 1.000000000000000000 ) ) 
 REPRESENTATION_ITEM ( '' )  );
#5621 = VERTEX_POINT ( 'NONE', #2533 ) ;
#5622 = CARTESIAN_POINT ( 'NONE',  ( 5.722153740306476166, 44.16218185472587976, 94.89411094854372664 ) ) ;
#5623 = CARTESIAN_POINT ( 'NONE',  ( 25.63948732994507651, 36.35905713404684292, 74.70433879953100131 ) ) ;
#5624 = EDGE_CURVE ( 'NONE', #10630, #8638, #4407, .T. ) ;
#5625 = DIRECTION ( 'NONE',  ( 0.6080936526121348829, 0.7938652969193402686, 2.360290325043241787E-16 ) ) ;
#5626 = CARTESIAN_POINT ( 'NONE',  ( 5.568489401881125289, 48.03437091500646261, 95.57058880123798872 ) ) ;
#5627 = PLANE ( 'NONE',  #13602 ) ;
#5628 = CARTESIAN_POINT ( 'NONE',  ( -7.520603205048787210, 47.87625257981667914, 78.82648837639791850 ) ) ;
#5629 = DIRECTION ( 'NONE',  ( 0.3165065846431827645, 0.9485903129789529098, 0.000000000000000000 ) ) ;
#5630 = CARTESIAN_POINT ( 'NONE',  ( 5.542130322670884013, 50.64142601547019495, 78.27786821129558348 ) ) ;
#5631 = ORIENTED_EDGE ( 'NONE', *, *, #13895, .F. ) ;
#5632 = ORIENTED_EDGE ( 'NONE', *, *, #17554, .T. ) ;
#5633 = CARTESIAN_POINT ( 'NONE',  ( 6.377548835851594156, 49.90291338712703606, 77.49502509244548776 ) ) ;
#5634 = CARTESIAN_POINT ( 'NONE',  ( 11.22215374030650281, 42.96218137147968008, 66.20574467885104752 ) ) ;
#5635 = LINE ( 'NONE', #18622, #16400 ) ;
#5636 = CARTESIAN_POINT ( 'NONE',  ( 0.5221537403065077410, 44.16218137147969713, 66.55433879953099563 ) ) ;
#5637 = CYLINDRICAL_SURFACE ( 'NONE', #11159, 4.200000000000000178 ) ;
#5638 = CARTESIAN_POINT ( 'NONE',  ( 5.544968037009670780, 45.50804040601273925, 91.19558880294498238 ) ) ;
#5639 = CARTESIAN_POINT ( 'NONE',  ( -0.1811115068269047168, 52.93481103811284783, 79.44677385717197637 ) ) ;
#5640 = CARTESIAN_POINT ( 'NONE',  ( -7.727133660016102468, 47.23791965223615819, 77.68791732120209304 ) ) ;
#5641 = CARTESIAN_POINT ( 'NONE',  ( 6.198496396448986090, 45.68315280215533392, 90.33621380123798872 ) ) ;
#5642 = B_SPLINE_SURFACE_WITH_KNOTS ( 'NONE', 3, 1, ( 
 ( #11383, #14658 ),
 ( #6566, #3792 ),
 ( #5378, #14010 ),
 ( #13696, #12106 ),
 ( #8703, #12010 ),
 ( #10739, #18481 ),
 ( #2307, #20269 ),
 ( #11897, #20062 ),
 ( #5601, #5815 ),
 ( #7194, #13581 ),
 ( #9022, #18374 ) ),
 .UNSPECIFIED., .F., .F., .F.,
 ( 4, 1, 1, 1, 1, 1, 1, 1, 4 ),
 ( 2, 2 ),
 ( 0.000000000000000000, 0.1183643824554993229, 0.2230508441810244713, 0.3193022156518771082, 0.4115690293017447154, 0.5153686147994278599, 0.6444437064119312719, 0.8055807690274368049, 1.000000000000000000 ),
 ( 0.000000000000000000, 1.000000000000000000 ),
 .UNSPECIFIED. ) ;
#5643 = DIRECTION ( 'NONE',  ( 1.540237394707284220E-16, 1.793354297423764243E-16, -1.000000000000000000 ) ) ;
#5644 = VERTEX_POINT ( 'NONE', #2944 ) ;
#5645 = CARTESIAN_POINT ( 'NONE',  ( 5.939900590116411472, 51.10072461867315496, 76.90580938776616904 ) ) ;
#5646 = ORIENTED_EDGE ( 'NONE', *, *, #20564, .T. ) ;
#5647 = CARTESIAN_POINT ( 'NONE',  ( -4.799400614414246036, 51.17536568166803335, 78.65631888207801126 ) ) ;
#5648 = CARTESIAN_POINT ( 'NONE',  ( -4.567115856812060670, 47.10047254335474065, 93.30496380123798872 ) ) ;
#5649 = VERTEX_POINT ( 'NONE', #10949 ) ;
#5650 = CARTESIAN_POINT ( 'NONE',  ( -4.812088799398940075, 42.22067586467031930, 93.96996379782397923 ) ) ;
#5651 = B_SPLINE_CURVE_WITH_KNOTS ( 'NONE', 3,
 ( #20129, #7154, #15256, #18549, #672, #10596, #5566, #18764, #883, #13758, #13543, #20229, #16850, #11965, #9087 ),
 .UNSPECIFIED., .F., .F.,
 ( 4, 1, 1, 1, 1, 1, 1, 1, 1, 1, 1, 1, 4 ),
 ( 0.000000000000000000, 0.1372453196419673171, 0.2656077965333414337, 0.3855481208555507355, 0.4976308828580581767, 0.5516434046647483713, 0.6057582083304485776, 0.6621535423365251249, 0.7211227168729713588, 0.7835375577407022174, 0.8505035567791932039, 0.9228138635028276804, 1.000000000000000000 ),
 .UNSPECIFIED. ) ;
#5652 = CARTESIAN_POINT ( 'NONE',  ( 4.100190290135135029, 51.54036911970691648, 72.45433879953087342 ) ) ;
#5653 = VECTOR ( 'NONE', #12759, 1000.000000000000000 ) ;
#5654 = CARTESIAN_POINT ( 'NONE',  ( -3.405315259844419185, 52.17152803532113126, 78.78030711080756987 ) ) ;
#5655 = CARTESIAN_POINT ( 'NONE',  ( 0.8503282811412333775, 52.95606000782370870, 77.76169174070734869 ) ) ;
#5656 = CARTESIAN_POINT ( 'NONE',  ( 5.200734800563608928, 50.89208066999871249, 76.90580938776616904 ) ) ;
#5657 = CARTESIAN_POINT ( 'NONE',  ( -3.198686620050343876, 36.88421666131827692, 79.01720576857120193 ) ) ;
#5658 = ORIENTED_EDGE ( 'NONE', *, *, #8351, .T. ) ;
#5659 = CARTESIAN_POINT ( 'NONE',  ( 4.019338295582739029, 36.74531179668952774, 78.10496264922831244 ) ) ;
#5660 = EDGE_CURVE ( 'NONE', #18556, #20977, #20599, .T. ) ;
#5661 = ORIENTED_EDGE ( 'NONE', *, *, #16128, .F. ) ;
#5662 = CARTESIAN_POINT ( 'NONE',  ( -4.205066710492285864, 37.45915809019812315, 75.36189689747067177 ) ) ;
#5663 = CARTESIAN_POINT ( 'NONE',  ( 0.5221537403065005245, 44.16218137147968292, 82.45433879953087342 ) ) ;
#5664 = CARTESIAN_POINT ( 'NONE',  ( 5.898472913175941024, 51.13132557482045826, 79.54598470662274678 ) ) ;
#5665 = CARTESIAN_POINT ( 'NONE',  ( -4.517072128342571880, 36.94403992325788977, 78.34992703482498655 ) ) ;
#5666 = CARTESIAN_POINT ( 'NONE',  ( 4.673174852049363004, 39.63213674411673537, 91.86058879782397923 ) ) ;
#5667 = CARTESIAN_POINT ( 'NONE',  ( 5.541475489004265675, 50.64875218668856860, 79.54599097325484536 ) ) ;
#5668 = AXIS2_PLACEMENT_3D ( 'NONE', #20339, #11181, #15571 ) ;
#5669 = ORIENTED_EDGE ( 'NONE', *, *, #12657, .F. ) ;
#5670 = CARTESIAN_POINT ( 'NONE',  ( 5.631785411401764918, 36.99756487055721976, 77.76022115247205591 ) ) ;
#5671 = ORIENTED_EDGE ( 'NONE', *, *, #13786, .F. ) ;
#5672 = DIRECTION ( 'NONE',  ( -0.9485903129789527988, 0.3165065846431829311, -8.934458285744989980E-17 ) ) ;
#5673 = CARTESIAN_POINT ( 'NONE',  ( -5.058133621542618030, 44.89684013992257405, 92.67996379953099506 ) ) ;
#5674 = VERTEX_POINT ( 'NONE', #6236 ) ;
#5675 = CARTESIAN_POINT ( 'NONE',  ( 6.828503391016846891, 43.33193468930419101, 95.41433880123797451 ) ) ;
#5676 = DIRECTION ( 'NONE',  ( 1.000000000000000000, 0.000000000000000000, 0.000000000000000000 ) ) ;
#5677 = CARTESIAN_POINT ( 'NONE',  ( 3.051792653884171536, 39.75632934307087396, 95.05433879953095300 ) ) ;
#5678 = CARTESIAN_POINT ( 'NONE',  ( -4.777409764772176715, 51.19107953768585872, 78.82882669246485818 ) ) ;
#5679 = CARTESIAN_POINT ( 'NONE',  ( 3.948530577815480225, 39.69684013992245752, 91.89871379953099506 ) ) ;
#5680 = ORIENTED_EDGE ( 'NONE', *, *, #3505, .F. ) ;
#5681 = CARTESIAN_POINT ( 'NONE',  ( 0.8388999841772379895, 52.35664863430569937, 79.54465842518074226 ) ) ;
#5682 = CARTESIAN_POINT ( 'NONE',  ( -5.784195910403845176, 44.99242805365518194, 96.03933880123796030 ) ) ;
#5683 = VECTOR ( 'NONE', #14854, 1000.000000000000000 ) ;
#5684 = ADVANCED_FACE ( 'NONE', ( #8052 ), #680, .F. ) ;
#5685 = ORIENTED_EDGE ( 'NONE', *, *, #20566, .T. ) ;
#5686 = DIRECTION ( 'NONE',  ( 0.007885122365275720746, 0.9999689119394086223, 1.805443505845543882E-16 ) ) ;
#5687 = DIRECTION ( 'NONE',  ( 1.540237394707284220E-16, 1.793354297423764243E-16, -1.000000000000000000 ) ) ;
#5688 = LINE ( 'NONE', #12196, #3848 ) ;
#5689 = PRODUCT_CONTEXT ( 'NONE', #4361, 'mechanical' ) ;
#5690 = CARTESIAN_POINT ( 'NONE',  ( -4.534424312541050384, 37.71149322473957000, 76.32271929704664615 ) ) ;
#5691 = DIRECTION ( 'NONE',  ( -1.402518428993831183E-16, 1.000000000000000000, -3.469446951953617640E-16 ) ) ;
#5692 = VECTOR ( 'NONE', #2971, 1000.000000000000000 ) ;
#5693 = CARTESIAN_POINT ( 'NONE',  ( -7.390568127015174404, 42.00488250642126786, 77.49325708768887466 ) ) ;
#5694 = EDGE_CURVE ( 'NONE', #11086, #20176, #1548, .T. ) ;
#5695 = EDGE_LOOP ( 'NONE', ( #14844, #11281, #1974, #5170, #17695 ) ) ;
#5696 = CARTESIAN_POINT ( 'NONE',  ( 2.038089102302941047, 52.95496222620524662, 76.00457246026148539 ) ) ;
#5697 = ADVANCED_FACE ( 'NONE', ( #1465 ), #14333, .F. ) ;
#5698 = EDGE_LOOP ( 'NONE', ( #3918, #13267, #20700, #13360 ) ) ;
#5699 = CARTESIAN_POINT ( 'NONE',  ( 6.960985561621730433, 50.34649028203376275, 76.51259071708746262 ) ) ;
#5700 = CARTESIAN_POINT ( 'NONE',  ( -5.368445182934982185, 36.96218137147968008, 80.55433879953099563 ) ) ;
#5701 = CARTESIAN_POINT ( 'NONE',  ( 3.460444912181559474, 49.25145096859824889, 90.64871380123798872 ) ) ;
#5702 = ORIENTED_EDGE ( 'NONE', *, *, #9013, .T. ) ;
#5703 = ADVANCED_FACE ( 'NONE', ( #20904 ), #12253, .T. ) ;
#5704 = CARTESIAN_POINT ( 'NONE',  ( 5.934911976351838092, 50.19039450147929671, 79.44748646226150868 ) ) ;
#5705 = ORIENTED_EDGE ( 'NONE', *, *, #2105, .F. ) ;
#5706 = LINE ( 'NONE', #9133, #14533 ) ;
#5707 = ADVANCED_FACE ( 'NONE', ( #1356 ), #12937, .F. ) ;
#5708 = CARTESIAN_POINT ( 'NONE',  ( 2.246318977524932148, 38.35943151540528362, 72.45432679953087529 ) ) ;
#5709 = CARTESIAN_POINT ( 'NONE',  ( -4.009385194876760927, 46.27527268018315709, 92.01683879953097289 ) ) ;
#5710 = ADVANCED_FACE ( 'NONE', ( #14850 ), #6655, .T. ) ;
#5711 = AXIS2_PLACEMENT_3D ( 'NONE', #20999, #6434, #13151 ) ;
#5712 = CARTESIAN_POINT ( 'NONE',  ( 5.394152393224890041, 50.75790946820724514, 75.36022115247205022 ) ) ;
#5714 = EDGE_CURVE ( 'NONE', #3020, #13327, #6863, .T. ) ;
#5713 = CARTESIAN_POINT ( 'NONE',  ( -5.917125461193805336, 40.64525615903904310, 75.45433879953087342 ) ) ;
#5715 = CARTESIAN_POINT ( 'NONE',  ( -7.435644857393074680, 42.18194711778849637, 79.51259448158572241 ) ) ;
#5716 = DIRECTION ( 'NONE',  ( 1.540237394707284220E-16, 1.793354297423764243E-16, -1.000000000000000000 ) ) ;
#5717 = CARTESIAN_POINT ( 'NONE',  ( 0.5221537403065008576, 44.16218137147968292, 80.45433879953087342 ) ) ;
#5718 = CARTESIAN_POINT ( 'NONE',  ( -5.754662135367683895, 50.49277077315122142, 75.98690818113186651 ) ) ;
#5719 = CARTESIAN_POINT ( 'NONE',  ( 4.801502123416836021, 51.01678076155011610, 75.41617184184443090 ) ) ;
#5720 = EDGE_CURVE ( 'NONE', #5251, #1145, #13057, .T. ) ;
#5721 = CARTESIAN_POINT ( 'NONE',  ( -4.500660556396669065, 42.81632233694663370, 94.32058880294496817 ) ) ;
#5722 = CARTESIAN_POINT ( 'NONE',  ( -7.956811444893308938, 41.77663113577187204, 78.52713215918005574 ) ) ;
#5723 = FACE_OUTER_BOUND ( 'NONE', #3371, .T. ) ;
#5724 = AXIS2_PLACEMENT_3D ( 'NONE', #12271, #20218, #16631 ) ;
#5725 = VERTEX_POINT ( 'NONE', #8585 ) ;
#5726 = LINE ( 'NONE', #17123, #18332 ) ;
#5727 = DIRECTION ( 'NONE',  ( -0.3014917755252044529, 0.9534116768940187336, -0.01043473300065710097 ) ) ;
#5728 = DIRECTION ( 'NONE',  ( -1.000000000000000000, 0.000000000000000000, 0.000000000000000000 ) ) ;
#5729 = CARTESIAN_POINT ( 'NONE',  ( -5.784195910403845176, 44.99242805365518194, 96.03933880123796030 ) ) ;
#5730 = DIRECTION ( 'NONE',  ( -0.000000000000000000, -0.000000000000000000, 1.000000000000000000 ) ) ;
#5731 = CARTESIAN_POINT ( 'NONE',  ( -7.607017829814316734, 43.12095717434316100, 78.33204358585338412 ) ) ;
#5732 = CARTESIAN_POINT ( 'NONE',  ( 8.443422548343662015, 42.04239353520513589, 78.13669174070733447 ) ) ;
#5733 = PLANE ( 'NONE',  #15287 ) ;
#5734 = ORIENTED_EDGE ( 'NONE', *, *, #18091, .F. ) ;
#5735 = EDGE_LOOP ( 'NONE', ( #2636, #17920, #14112, #20862, #12809 ) ) ;
#5736 = PRODUCT_DEFINITION_CONTEXT ( 'detailed design', #5874, 'design' ) ;
#5737 = CARTESIAN_POINT ( 'NONE',  ( 9.318068138769051600, 42.72056584129816059, 78.97126489842982267 ) ) ;
#5739 = EDGE_CURVE ( 'NONE', #8576, #8218, #6112, .T. ) ;
#5738 = CARTESIAN_POINT ( 'NONE',  ( -3.872497565881518611, 36.46791865901509766, 75.57130654555172100 ) ) ;
#5740 = CARTESIAN_POINT ( 'NONE',  ( -4.477846259693478714, 37.66295064777091994, 53.55433879953098852 ) ) ;
#5741 = CARTESIAN_POINT ( 'NONE',  ( 5.939883047636084434, 51.10073757659671401, 76.92469047792664583 ) ) ;
#5742 = CARTESIAN_POINT ( 'NONE',  ( -3.857995858694130753, 47.10914555767435274, 95.05433879953105247 ) ) ;
#5743 = VECTOR ( 'NONE', #11956, 999.9999999999998863 ) ;
#5744 = CARTESIAN_POINT ( 'NONE',  ( 8.491425378215518904, 42.60748309719328830, 78.02362291919803283 ) ) ;
#5745 = CARTESIAN_POINT ( 'NONE',  ( 3.122153740306552905, 48.66551347115873227, 92.60183880294498238 ) ) ;
#5746 = EDGE_CURVE ( 'NONE', #20489, #3856, #1670, .T. ) ;
#5747 = CARTESIAN_POINT ( 'NONE',  ( -5.784195910403845176, 44.99242805365518194, 93.38308880123798872 ) ) ;
#5748 =( BOUNDED_CURVE ( )  B_SPLINE_CURVE ( 3, ( #460, #15469, #6941, #5342 ),
 .UNSPECIFIED., .F., .F. ) 
 B_SPLINE_CURVE_WITH_KNOTS ( ( 4, 4 ),
 ( 1.414584307249941553, 1.415673517910795987 ),
 .UNSPECIFIED. ) 
 CURVE ( )  GEOMETRIC_REPRESENTATION_ITEM ( )  RATIONAL_B_SPLINE_CURVE ( ( 1.000000000000000000, 0.9999999011350138023, 0.9999999011350138023, 1.000000000000000000 ) ) 
 REPRESENTATION_ITEM ( '' )  );
#5749 = CARTESIAN_POINT ( 'NONE',  ( -4.385532207686900996, 51.47110089242590902, 76.31459635612003467 ) ) ;
#5750 = AXIS2_PLACEMENT_3D ( 'NONE', #8485, #390, #14971 ) ;
#5751 = CARTESIAN_POINT ( 'NONE',  ( 4.167070027254266229, 47.87117560886914447, 95.05212442257573002 ) ) ;
#5752 = CARTESIAN_POINT ( 'NONE',  ( -3.350035803220276609, 49.20851703305431357, 91.97683880123797451 ) ) ;
#5753 = VECTOR ( 'NONE', #4728, 1000.000000000000227 ) ;
#5754 = CARTESIAN_POINT ( 'NONE',  ( 6.490738213730996797, 37.61134109483241872, 75.55565825109377442 ) ) ;
#5755 = ORIENTED_EDGE ( 'NONE', *, *, #13413, .F. ) ;
#5756 = EDGE_CURVE ( 'NONE', #20991, #13992, #1980, .T. ) ;
#5757 = DIRECTION ( 'NONE',  ( 1.540237394707284220E-16, 1.793354297423764243E-16, -1.000000000000000000 ) ) ;
#5758 = CIRCLE ( 'NONE', #19347, 1.399999999999995026 ) ;
#5759 = VERTEX_POINT ( 'NONE', #9870 ) ;
#5760 = CARTESIAN_POINT ( 'NONE',  ( -4.432065751971962619, 50.69093429316135513, 78.79723525346945223 ) ) ;
#5761 = CARTESIAN_POINT ( 'NONE',  ( 5.611423337425062385, 41.22389019960463230, 90.17996380123798872 ) ) ;
#5762 = VERTEX_POINT ( 'NONE', #17939 ) ;
#5763 = DIRECTION ( 'NONE',  ( -1.110223024625156540E-16, -1.000000000000000000, -5.922860397471808077E-17 ) ) ;
#5765 = VECTOR ( 'NONE', #12429, 1000.000000000000000 ) ;
#5764 = PLANE ( 'NONE',  #5724 ) ;
#5766 = AXIS2_PLACEMENT_3D ( 'NONE', #8507, #14992, #5289 ) ;
#5767 = CARTESIAN_POINT ( 'NONE',  ( -3.363202728395832342, 52.20162010845611178, 78.48078762820125576 ) ) ;
#5768 = DIRECTION ( 'NONE',  ( 3.154042683594179047E-15, 4.423602989573997160E-31, -1.000000000000000000 ) ) ;
#5769 = CARTESIAN_POINT ( 'NONE',  ( 5.561379608955574483, 51.38032281970146897, 76.90580938776616904 ) ) ;
#5770 = DIRECTION ( 'NONE',  ( -1.779391786395883536E-16, -5.922860397471806844E-17, 1.000000000000000000 ) ) ;
#5771 = ORIENTED_EDGE ( 'NONE', *, *, #20663, .F. ) ;
#5772 = CYLINDRICAL_SURFACE ( 'NONE', #3070, 8.799999999999995381 ) ;
#5773 = CARTESIAN_POINT ( 'NONE',  ( -5.616286711741429905, 44.43019146960381960, 92.48558879782397923 ) ) ;
#5774 = VERTEX_POINT ( 'NONE', #8474 ) ;
#5775 = DIRECTION ( 'NONE',  ( -1.402518428993830937E-16, 1.000000000000000000, -3.469446951953617147E-16 ) ) ;
#5776 = CARTESIAN_POINT ( 'NONE',  ( 11.22215374030650281, 42.96218137147968008, 57.80715055817105252 ) ) ;
#5777 = LINE ( 'NONE', #12386, #2654 ) ;
#5778 = AXIS2_PLACEMENT_3D ( 'NONE', #20049, #7294, #18674 ) ;
#5779 = VECTOR ( 'NONE', #19413, 1000.000000000000000 ) ;
#5780 = DIRECTION ( 'NONE',  ( 1.000000000000000000, 1.402518428993831676E-16, 0.000000000000000000 ) ) ;
#5781 = CARTESIAN_POINT ( 'NONE',  ( -7.332874749269493009, 40.19484192575331605, 78.03982737165262051 ) ) ;
#5782 = CARTESIAN_POINT ( 'NONE',  ( 3.099655065065782367, 37.00631057046153671, 72.45433879953085921 ) ) ;
#5783 = CARTESIAN_POINT ( 'NONE',  ( -4.202939935851639497, 37.46040681653102666, 78.03811350732550522 ) ) ;
#5784 = CARTESIAN_POINT ( 'NONE',  ( 6.443166240752919549, 49.83520380470869071, 78.90732027998019760 ) ) ;
#5785 = B_SPLINE_SURFACE_WITH_KNOTS ( 'NONE', 3, 1, ( 
 ( #19501, #3546 ),
 ( #6834, #16530 ),
 ( #42, #1641 ),
 ( #18225, #346 ),
 ( #3643, #10156 ),
 ( #5129, #9950 ),
 ( #19709, #11750 ),
 ( #8233, #14721 ),
 ( #11648, #13232 ),
 ( #14921, #6728 ),
 ( #11436, #16324 ),
 ( #1950, #4813 ),
 ( #6621, #8441 ),
 ( #141, #18127 ),
 ( #16636, #13340 ) ),
 .UNSPECIFIED., .F., .F., .F.,
 ( 4, 1, 1, 1, 1, 1, 1, 1, 1, 1, 1, 1, 4 ),
 ( 2, 2 ),
 ( 0.000000000000000000, 0.1267531625455885769, 0.2402085644777646467, 0.3404273024139109483, 0.4286057740769950719, 0.5026654758471001960, 0.5652545264784208934, 0.6141369997546152204, 0.6524264903941315863, 0.7200380101346053330, 0.7961149349448265466, 0.8886173437222998350, 0.9999999999999998890 ),
 ( 0.000000000000000000, 1.000000000000000000 ),
 .UNSPECIFIED. ) ;
#5786 = AXIS2_PLACEMENT_3D ( 'NONE', #14380, #12784, #19266 ) ;
#5787 = ORIENTED_EDGE ( 'NONE', *, *, #6660, .T. ) ;
#5788 = FACE_OUTER_BOUND ( 'NONE', #14179, .T. ) ;
#5789 = VERTEX_POINT ( 'NONE', #6959 ) ;
#5790 = CARTESIAN_POINT ( 'NONE',  ( 27.03948732994508930, 45.16218137147969003, 78.30433879953100984 ) ) ;
#5791 = CARTESIAN_POINT ( 'NONE',  ( -3.943187491250720544, 40.73580453397070755, 92.83621379953099506 ) ) ;
#5792 = VECTOR ( 'NONE', #18183, 1000.000000000000000 ) ;
#5793 = ORIENTED_EDGE ( 'NONE', *, *, #14285, .F. ) ;
#5794 = CARTESIAN_POINT ( 'NONE',  ( -3.350035803220276609, 49.20851703305431357, 93.38308880123798872 ) ) ;
#5795 = FACE_BOUND ( 'NONE', #4053, .T. ) ;
#5796 = LINE ( 'NONE', #7060, #17622 ) ;
#5797 = CARTESIAN_POINT ( 'NONE',  ( -4.744888236371026302, 51.21431823119217341, 78.89490084226201816 ) ) ;
#5798 = VERTEX_POINT ( 'NONE', #19737 ) ;
#5799 = CARTESIAN_POINT ( 'NONE',  ( 0.5221537403065019678, 44.16218137147968292, 72.45433879953087342 ) ) ;
#5800 = CARTESIAN_POINT ( 'NONE',  ( -3.350035803220276609, 49.20851703305431357, 90.88308880123797451 ) ) ;
#5801 = AXIS2_PLACEMENT_3D ( 'NONE', #5406, #15216, #627 ) ;
#5802 = ORIENTED_EDGE ( 'NONE', *, *, #5425, .F. ) ;
#5803 = CARTESIAN_POINT ( 'NONE',  ( -4.639915919080545237, 42.28775865649100041, 92.45433879953091605 ) ) ;
#5804 = CARTESIAN_POINT ( 'NONE',  ( 5.077393176519246154, 37.34383885640306033, 76.55500641741416246 ) ) ;
#5805 = APPLICATION_PROTOCOL_DEFINITION ( 'draft international standard', 'automotive_design', 1998, #14284 ) ;
#5806 = CARTESIAN_POINT ( 'NONE',  ( 5.449567083428624947, 36.86735832482640518, 76.18683980367092090 ) ) ;
#5807 = CARTESIAN_POINT ( 'NONE',  ( 5.713366999337934793, 51.26805585685155364, 78.93442753446957738 ) ) ;
#5808 = LINE ( 'NONE', #18896, #19778 ) ;
#5809 = ORIENTED_EDGE ( 'NONE', *, *, #2882, .F. ) ;
#5810 = EDGE_CURVE ( 'NONE', #3928, #2511, #19936, .T. ) ;
#5811 = DIRECTION ( 'NONE',  ( 0.007885122365275663500, 0.9999689119394085113, 1.805443505845543142E-16 ) ) ;
#5812 = B_SPLINE_CURVE_WITH_KNOTS ( 'NONE', 3,
 ( #14296, #7610, #11226, #12499, #9322, #14093, #14504, #9630, #20872, #16112 ),
 .UNSPECIFIED., .F., .F.,
 ( 4, 2, 2, 2, 4 ),
 ( 0.000000000000000000, 0.001160160651305680753, 0.002320321302611361072, 0.003480481953917041391, 0.004640642605222721276 ),
 .UNSPECIFIED. ) ;
#5813 = EDGE_LOOP ( 'NONE', ( #17302, #15190, #8651, #2137, #11528 ) ) ;
#5814 = CARTESIAN_POINT ( 'NONE',  ( -0.2981274494836149147, 52.32174374914394122, 79.40375978592670947 ) ) ;
#5815 = CARTESIAN_POINT ( 'NONE',  ( 0.3342292354559211476, 52.96756143588948618, 77.66452874556115660 ) ) ;
#5816 = CARTESIAN_POINT ( 'NONE',  ( -2.416137431568557314, 39.07291177436112406, 92.52371380123797451 ) ) ;
#5817 = LINE ( 'NONE', #18803, #17408 ) ;
#5818 = ORIENTED_EDGE ( 'NONE', *, *, #13819, .T. ) ;
#5819 = CARTESIAN_POINT ( 'NONE',  ( 10.77494014480653917, 42.96218137147968008, 57.80715055817105252 ) ) ;
#5820 = VECTOR ( 'NONE', #5643, 1000.000000000000000 ) ;
#5821 = ORIENTED_EDGE ( 'NONE', *, *, #8407, .T. ) ;
#5822 = LINE ( 'NONE', #10641, #19626 ) ;
#5823 = CARTESIAN_POINT ( 'NONE',  ( 5.427780505986065762, 36.85179043424346190, 76.96022115247204454 ) ) ;
#5824 = CARTESIAN_POINT ( 'NONE',  ( 7.670935877285506521, 40.16519072103186261, 76.98031643592585738 ) ) ;
#5825 = ADVANCED_FACE ( 'NONE', ( #18153 ), #16666, .F. ) ;
#5826 = CARTESIAN_POINT ( 'NONE',  ( 5.320112028679005789, 37.51224306767437611, 77.75838138190746918 ) ) ;
#5827 = CARTESIAN_POINT ( 'NONE',  ( -6.930444918848789548, 41.01030821858960707, 79.43600262374511090 ) ) ;
#5828 = LINE ( 'NONE', #9251, #427 ) ;
#5829 = CARTESIAN_POINT ( 'NONE',  ( 6.828503391016846891, 43.33193468930419101, 95.41433880123797451 ) ) ;
#5830 = CARTESIAN_POINT ( 'NONE',  ( -3.944959226007137776, 38.51060946023304865, 78.53742703482498655 ) ) ;
#5831 = CARTESIAN_POINT ( 'NONE',  ( 0.6120586831527303762, 52.96175337023965568, 78.93565972088759963 ) ) ;
#5832 = CARTESIAN_POINT ( 'NONE',  ( 4.881482038019723468, 51.88253576740703465, 75.58280986828056314 ) ) ;
#5833 = CARTESIAN_POINT ( 'NONE',  ( 1.868012774839550749, 39.13936707477651566, 90.88308880294496817 ) ) ;
#5834 = EDGE_CURVE ( 'NONE', #13618, #17974, #15277, .T. ) ;
#5835 = VECTOR ( 'NONE', #4000, 999.9999999999998863 ) ;
#5836 = CARTESIAN_POINT ( 'NONE',  ( -7.319506999482564780, 40.16856015084685083, 78.85321517283955473 ) ) ;
#5837 = CARTESIAN_POINT ( 'NONE',  ( 11.22215374030650281, 42.76218137147968434, 72.80433879953100984 ) ) ;
#5838 = AXIS2_PLACEMENT_3D ( 'NONE', #9467, #11168, #12345 ) ;
#5839 = EDGE_CURVE ( 'NONE', #6821, #5209, #13563, .T. ) ;
#5840 = ORIENTED_EDGE ( 'NONE', *, *, #16017, .F. ) ;
#5841 = PLANE ( 'NONE',  #12227 ) ;
#5842 = FACE_OUTER_BOUND ( 'NONE', #18379, .T. ) ;
#5843 = CARTESIAN_POINT ( 'NONE',  ( -4.452164423840478946, 50.68111428912082772, 78.66650520056290929 ) ) ;
#5844 = LINE ( 'NONE', #11278, #11292 ) ;
#5845 = CARTESIAN_POINT ( 'NONE',  ( -4.806942593991912815, 37.15815555953845717, 77.31392376534303423 ) ) ;
#5846 = CARTESIAN_POINT ( 'NONE',  ( -8.203676112595456260, 42.55548883657580461, 79.26478910100486530 ) ) ;
#5847 = CARTESIAN_POINT ( 'NONE',  ( 8.513836386385465360, 42.32043698847956392, 78.11831813120640788 ) ) ;
#5848 = EDGE_CURVE ( 'NONE', #6944, #8267, #10725, .T. ) ;
#5849 = VERTEX_POINT ( 'NONE', #2289 ) ;
#5850 = EDGE_LOOP ( 'NONE', ( #8113, #10368, #6357, #388 ) ) ;
#5851 = VECTOR ( 'NONE', #15106, 1000.000000000000000 ) ;
#5852 = CARTESIAN_POINT ( 'NONE',  ( -4.469629189018287541, 37.65660658733380473, 78.89921164031883904 ) ) ;
#5853 = CARTESIAN_POINT ( 'NONE',  ( -3.568428810981484567, 36.24331531840702070, 78.81697279211699936 ) ) ;
#5854 = DIRECTION ( 'NONE',  ( 0.007885122365275663500, 0.9999689119394085113, 1.805443505845543142E-16 ) ) ;
#5855 = VECTOR ( 'NONE', #9054, 1000.000000000000000 ) ;
#5856 = LINE ( 'NONE', #16824, #10322 ) ;
#5857 = CARTESIAN_POINT ( 'NONE',  ( 8.889236131602293867, 41.43532911122410667, 77.52218233473911368 ) ) ;
#5858 = FACE_OUTER_BOUND ( 'NONE', #16092, .T. ) ;
#5859 = PLANE ( 'NONE',  #17263 ) ;
#5860 = CARTESIAN_POINT ( 'NONE',  ( 1.352400422481993658, 50.46853102219002096, 93.07058880123798872 ) ) ;
#5861 = CARTESIAN_POINT ( 'NONE',  ( -0.9388773962491537839, 52.84004908296358138, 77.77566232894263010 ) ) ;
#5862 = CARTESIAN_POINT ( 'NONE',  ( 31.22215374030650281, 42.76218137147968434, 78.80433879953099563 ) ) ;
#5863 = CARTESIAN_POINT ( 'NONE',  ( 3.122075258343615545, 38.59543968120053847, 90.05576841395854615 ) ) ;
#5864 = EDGE_CURVE ( 'NONE', #8749, #7909, #5343, .T. ) ;
#5865 = VECTOR ( 'NONE', #17019, 1000.000000000000000 ) ;
#5866 = CARTESIAN_POINT ( 'NONE',  ( 0.5838706545074757726, 52.36194911346490954, 78.93669174070734584 ) ) ;
#5867 = VERTEX_POINT ( 'NONE', #17088 ) ;
#5868 = ADVANCED_FACE ( 'NONE', ( #3878 ), #7290, .F. ) ;
#5869 = AXIS2_PLACEMENT_3D ( 'NONE', #933, #18597, #9140 ) ;
#5870 = CARTESIAN_POINT ( 'NONE',  ( 2.049637653786152036, 52.21875004887607474, 76.04051628124992135 ) ) ;
#5871 = ORIENTED_EDGE ( 'NONE', *, *, #8972, .F. ) ;
#5872 = CARTESIAN_POINT ( 'NONE',  ( -4.804534436424639843, 51.17169724042062739, 78.47639829077699858 ) ) ;
#5873 = EDGE_CURVE ( 'NONE', #1868, #8638, #10401, .T. ) ;
#5874 = APPLICATION_CONTEXT ( 'automotive_design' ) ;
#5875 = CARTESIAN_POINT ( 'NONE',  ( 4.987494971863720927, 47.58855820898865829, 92.52371380294498238 ) ) ;
#5876 = ORIENTED_EDGE ( 'NONE', *, *, #20426, .T. ) ;
#5877 = CARTESIAN_POINT ( 'NONE',  ( -10.17784625969349754, 51.36218137147968577, 54.55433879953098852 ) ) ;
#5878 = EDGE_CURVE ( 'NONE', #4650, #13095, #8788, .T. ) ;
#5879 = CARTESIAN_POINT ( 'NONE',  ( -0.9437706019779806832, 52.21950657494897285, 77.21536821129558348 ) ) ;
#5880 = CARTESIAN_POINT ( 'NONE',  ( 8.359840211550212175, 41.80355114555996465, 78.11862058389174024 ) ) ;
#5881 = PLANE ( 'NONE',  #7046 ) ;
#5882 = CARTESIAN_POINT ( 'NONE',  ( 5.210721989228209949, 50.88470353604066787, 77.09285305542944400 ) ) ;
#5883 = CARTESIAN_POINT ( 'NONE',  ( -4.374795797692404342, 37.75296113427494049, 79.54845644658969661 ) ) ;
#5884 = ORIENTED_EDGE ( 'NONE', *, *, #3217, .F. ) ;
#5885 = CARTESIAN_POINT ( 'NONE',  ( 5.649998448837412646, 37.01057924028687296, 77.75931883872233641 ) ) ;
#5886 = AXIS2_PLACEMENT_3D ( 'NONE', #4217, #1353, #11149 ) ;
#5887 = ORIENTED_EDGE ( 'NONE', *, *, #3709, .F. ) ;
#5888 = CARTESIAN_POINT ( 'NONE',  ( -4.359893715479207899, 37.57388776543446340, 75.36022115247205022 ) ) ;
#5889 = DIRECTION ( 'NONE',  ( 0.000000000000000000, 1.000000000000000000, 1.734723475976787531E-14 ) ) ;
#5890 = CARTESIAN_POINT ( 'NONE',  ( -4.567115856812060670, 47.10047254335474065, 95.80496380123798872 ) ) ;
#5891 = DIRECTION ( 'NONE',  ( -0.8136266022444372803, -0.5813877811927011807, -2.295812393977109100E-16 ) ) ;
#5892 = CARTESIAN_POINT ( 'NONE',  ( -4.159044950571627375, 37.42969452488605953, 78.30435701636687895 ) ) ;
#5893 = CARTESIAN_POINT ( 'NONE',  ( 5.225516393853212982, 37.44489119831073509, 78.25751643855714690 ) ) ;
#5894 = B_SPLINE_CURVE_WITH_KNOTS ( 'NONE', 3,
 ( #3106, #16090, #1513, #1099, #14269, #19073, #11003, #7788, #20451, #5885, #17474 ),
 .UNSPECIFIED., .F., .F.,
 ( 4, 1, 1, 1, 1, 1, 1, 1, 4 ),
 ( 0.000000000000000000, 0.1895954080786773355, 0.3480750146108056442, 0.4761617831461403827, 0.5797469728315796100, 0.6725800605763750939, 0.7701180849273350226, 0.8764776678571430946, 1.000000000000000000 ),
 .UNSPECIFIED. ) ;
#5895 = ORIENTED_EDGE ( 'NONE', *, *, #14085, .F. ) ;
#5896 = CARTESIAN_POINT ( 'NONE',  ( 1.514255888186008203, 51.36218137147968577, 52.53721119516358584 ) ) ;
#5897 = VERTEX_POINT ( 'NONE', #8687 ) ;
#5898 = VECTOR ( 'NONE', #4683, 1000.000000000000000 ) ;
#5899 = DIRECTION ( 'NONE',  ( 4.142850521348543581E-16, -5.922860397471813007E-17, 1.000000000000000000 ) ) ;
#5900 = EDGE_CURVE ( 'NONE', #889, #4602, #1073, .T. ) ;
#5901 = CARTESIAN_POINT ( 'NONE',  ( -2.416137431568557314, 39.07291177436112406, 96.27371380123797451 ) ) ;
#5902 = CARTESIAN_POINT ( 'NONE',  ( -7.813433995296899859, 41.31607707846453792, 78.28419725522122974 ) ) ;
#5903 = ORIENTED_EDGE ( 'NONE', *, *, #6533, .F. ) ;
#5904 = CARTESIAN_POINT ( 'NONE',  ( -5.784195910403845176, 44.99242805365518194, 93.53933880123797451 ) ) ;
#5905 = CARTESIAN_POINT ( 'NONE',  ( 5.666884522201894647, 41.76315400873614436, 94.28246379782397923 ) ) ;
#5906 = CARTESIAN_POINT ( 'NONE',  ( 0.5221537403064979710, 39.16218137147969003, 93.35386871425482980 ) ) ;
#5907 = VERTEX_POINT ( 'NONE', #13679 ) ;
#5908 = CARTESIAN_POINT ( 'NONE',  ( 6.799065290779627624, 37.83166033551658103, 77.90902863000688683 ) ) ;
#5909 = DIRECTION ( 'NONE',  ( 0.000000000000000000, 0.000000000000000000, -1.000000000000000000 ) ) ;
#5910 = EDGE_LOOP ( 'NONE', ( #14645, #9514, #17185, #18195 ) ) ;
#5911 = FACE_BOUND ( 'NONE', #2942, .T. ) ;
#5912 = CARTESIAN_POINT ( 'NONE',  ( 0.8019475441090054835, 52.96387723590659391, 78.82560697059345500 ) ) ;
#5913 = ORIENTED_EDGE ( 'NONE', *, *, #4035, .F. ) ;
#5914 = CARTESIAN_POINT ( 'NONE',  ( -4.921387819424644761, 43.10902840346005149, 92.45433879953098710 ) ) ;
#5915 = CARTESIAN_POINT ( 'NONE',  ( 23.03948732994508575, 43.16218137147968292, 76.90433879953101837 ) ) ;
#5916 = CARTESIAN_POINT ( 'NONE',  ( 0.7901638384306278740, 50.30062182352762079, 93.57933879782399345 ) ) ;
#5917 = AXIS2_PLACEMENT_3D ( 'NONE', #4380, #2803, #15888 ) ;
#5918 = CARTESIAN_POINT ( 'NONE',  ( 5.429213800673928780, 36.85281461415114279, 76.52220546472133833 ) ) ;
#5919 = CARTESIAN_POINT ( 'NONE',  ( 5.549530740019891439, 36.93878869392346331, 75.99415254657458263 ) ) ;
#5920 = CARTESIAN_POINT ( 'NONE',  ( 31.03948732994507864, 45.16218137147969003, 78.30433879953099563 ) ) ;
#5921 = ORIENTED_EDGE ( 'NONE', *, *, #9153, .F. ) ;
#5922 = CARTESIAN_POINT ( 'NONE',  ( 0.8476006048031659024, 52.21151155428714219, 75.36710396340995999 ) ) ;
#5923 = ORIENTED_EDGE ( 'NONE', *, *, #19042, .F. ) ;
#5924 = LINE ( 'NONE', #15296, #11211 ) ;
#5925 = CARTESIAN_POINT ( 'NONE',  ( -0.9436870690626151248, 52.23009998296728895, 77.21536821129558348 ) ) ;
#5926 = CARTESIAN_POINT ( 'NONE',  ( 6.198496396448986090, 45.68315280215533392, 90.49246380123798872 ) ) ;
#5927 = ORIENTED_EDGE ( 'NONE', *, *, #13949, .T. ) ;
#5928 = CARTESIAN_POINT ( 'NONE',  ( -7.261062830191108652, 41.57632160563495205, 76.33871209835143645 ) ) ;
#5929 = B_SPLINE_CURVE_WITH_KNOTS ( 'NONE', 3,
 ( #17520, #5928, #6233, #6025, #17617, #4432, #17417, #3049, #2843, #15831, #1242, #7736, #11259, #3570, #16040, #6652 ),
 .UNSPECIFIED., .F., .F.,
 ( 4, 2, 2, 2, 2, 2, 2, 4 ),
 ( 0.000000000000000000, 0.0007160198473685760534, 0.001432039694737152107, 0.001790049618421429671, 0.002148059542105707018, 0.002506069465789984366, 0.002685074427632146241, 0.002864079389474307250 ),
 .UNSPECIFIED. ) ;
#5930 = ORIENTED_EDGE ( 'NONE', *, *, #5944, .F. ) ;
#5931 = CARTESIAN_POINT ( 'NONE',  ( 5.086801335794131518, 51.73087467290688579, 79.44143248960128290 ) ) ;
#5932 = FACE_OUTER_BOUND ( 'NONE', #5698, .T. ) ;
#5933 = CARTESIAN_POINT ( 'NONE',  ( 7.720651971079942832, 40.31419300806396677, 75.89798363837520867 ) ) ;
#5934 = ORIENTED_EDGE ( 'NONE', *, *, #14197, .T. ) ;
#5935 = DIRECTION ( 'NONE',  ( 0.000000000000000000, 0.000000000000000000, 1.000000000000000000 ) ) ;
#5936 = CARTESIAN_POINT ( 'NONE',  ( -7.733416094750764636, 41.06364772483073011, 79.50989352969267543 ) ) ;
#5937 = CARTESIAN_POINT ( 'NONE',  ( -5.945795452124602143, 37.96218137147967298, 95.05433879953098142 ) ) ;
#5938 = CARTESIAN_POINT ( 'NONE',  ( 3.788215052820487205, 39.19523464621513398, 90.24306233796824017 ) ) ;
#5939 = CARTESIAN_POINT ( 'NONE',  ( 2.522153740306511072, 50.16218137147969713, 53.15433879953100416 ) ) ;
#5940 = EDGE_CURVE ( 'NONE', #4901, #9713, #20044, .T. ) ;
#5941 = CARTESIAN_POINT ( 'NONE',  ( -1.440187084481237445, 38.28092143101015665, 78.25433879953088478 ) ) ;
#5942 = CARTESIAN_POINT ( 'NONE',  ( 1.868012774839550749, 39.13936707477651566, 94.63308880294498238 ) ) ;
#5943 = CARTESIAN_POINT ( 'NONE',  ( -5.667418469993653396, 43.80274312437727247, 78.25433879953087057 ) ) ;
#5944 = EDGE_CURVE ( 'NONE', #17793, #13982, #5583, .T. ) ;
#5945 = LINE ( 'NONE', #18923, #13318 ) ;
#5946 = CARTESIAN_POINT ( 'NONE',  ( 8.385938212755766230, 39.92691331981644254, 77.86095545630369941 ) ) ;
#5947 = B_SPLINE_CURVE_WITH_KNOTS ( 'NONE', 3,
 ( #16397, #13091, #3607, #6585, #8305, #16812, #19777, #11718, #18189, #421, #16598, #19565, #2019, #6906, #14785, #3820 ),
 .UNSPECIFIED., .F., .F.,
 ( 4, 2, 2, 2, 2, 2, 2, 4 ),
 ( 0.000000000000000000, 0.0005979303682485993549, 0.0008968955523729210417, 0.001195860736497242728, 0.001494825920621564632, 0.001793791104745886102, 0.002092756288870208006, 0.002391721472994529692 ),
 .UNSPECIFIED. ) ;
#5948 = CARTESIAN_POINT ( 'NONE',  ( -7.908914151385613600, 41.62335894602711051, 79.54737348031042643 ) ) ;
#5949 = CARTESIAN_POINT ( 'NONE',  ( 0.5221537403065019678, 44.16218137147968292, 72.45433879953087342 ) ) ;
#5950 = ORIENTED_EDGE ( 'NONE', *, *, #3626, .F. ) ;
#5951 = LINE ( 'NONE', #12450, #5653 ) ;
#5952 = DIRECTION ( 'NONE',  ( -0.02533578529877749536, -0.9996789974703350623, -1.831801750099157041E-16 ) ) ;
#5953 = CARTESIAN_POINT ( 'NONE',  ( 31.22215374030650281, 42.96218137147968008, 74.20433879953100131 ) ) ;
#5954 = CARTESIAN_POINT ( 'NONE',  ( 5.894741035747108171, 51.13408216234794423, 77.22227766523002401 ) ) ;
#5955 = B_SPLINE_SURFACE_WITH_KNOTS ( 'NONE', 3, 1, ( 
 ( #13844, #20440 ),
 ( #5872, #12156 ),
 ( #11950, #20114 ),
 ( #15558, #4050 ),
 ( #5647, #10578 ),
 ( #868, #9069 ),
 ( #4259, #2673 ),
 ( #3844, #5760 ),
 ( #7138, #15452 ),
 ( #2474, #7352 ),
 ( #12267, #10471 ),
 ( #3947, #657 ),
 ( #18747, #13638 ),
 ( #17150, #8753 ),
 ( #17250, #20324 ) ),
 .UNSPECIFIED., .F., .F., .F.,
 ( 4, 1, 1, 1, 1, 1, 1, 1, 1, 1, 1, 1, 4 ),
 ( 2, 2 ),
 ( 0.000000000000000000, 0.1198978896105060005, 0.2272848286615199442, 0.3233685559759303385, 0.4081414772668706115, 0.4819378103613651820, 0.5435227337441967954, 0.5948163272532476231, 0.6357474925148977052, 0.7079723711143988130, 0.7877128652614201476, 0.8832591045952046249, 1.000000000000000000 ),
 ( 0.000000000000000000, 1.000000000000000000 ),
 .UNSPECIFIED. ) ;
#5956 = CARTESIAN_POINT ( 'NONE',  ( 8.951667845840693971, 41.62244091939069790, 77.14698585835439815 ) ) ;
#5957 = CARTESIAN_POINT ( 'NONE',  ( -4.009385194876761815, 46.27527268018315709, 92.95433879611698558 ) ) ;
#5958 = DIRECTION ( 'NONE',  ( 1.110223024625156540E-16, 1.000000000000000000, 5.922860397471808077E-17 ) ) ;
#5959 = CARTESIAN_POINT ( 'NONE',  ( -0.9051307205072449680, 52.84566602866379981, 78.71653944640904399 ) ) ;
#5960 = ORIENTED_EDGE ( 'NONE', *, *, #19907, .T. ) ;
#5961 = CARTESIAN_POINT ( 'NONE',  ( 0.5981602388297567741, 52.96185312741366857, 75.36022115247205022 ) ) ;
#5962 = ADVANCED_FACE ( 'NONE', ( #8902, #5911, #13881, #15391, #804, #20252 ), #20363, .T. ) ;
#5963 = CARTESIAN_POINT ( 'NONE',  ( -3.677846259693482445, 44.16218137147969003, 56.15433879953099705 ) ) ;
#5964 = CARTESIAN_POINT ( 'NONE',  ( 5.873814141894775354, 51.14954001584995069, 78.86250487280319987 ) ) ;
#5965 = CARTESIAN_POINT ( 'NONE',  ( -4.804644443005473775, 51.17161863374555963, 78.45066232894264147 ) ) ;
#5966 = ORIENTED_EDGE ( 'NONE', *, *, #9221, .F. ) ;
#5967 = CARTESIAN_POINT ( 'NONE',  ( -7.677846259693479780, 44.16218137147969003, 53.55433879953099563 ) ) ;
#5968 = CARTESIAN_POINT ( 'NONE',  ( 4.987494971863720927, 47.58855820898865829, 93.77371380294498238 ) ) ;
#5969 = ORIENTED_EDGE ( 'NONE', *, *, #13793, .T. ) ;
#5970 = PLANE ( 'NONE',  #14716 ) ;
#5971 = DIRECTION ( 'NONE',  ( -0.000000000000000000, -1.000000000000000000, -0.000000000000000000 ) ) ;
#5972 = CARTESIAN_POINT ( 'NONE',  ( 8.804199926738755622, 41.18047021065184055, 77.88643322029270166 ) ) ;
#5973 = DIRECTION ( 'NONE',  ( -0.000000000000000000, -0.000000000000000000, 1.000000000000000000 ) ) ;
#5974 = DIRECTION ( 'NONE',  ( 0.5800177190770223756, 0.8146038580541392626, 2.354238310054622780E-16 ) ) ;
#5975 = CARTESIAN_POINT ( 'NONE',  ( -4.323846805489822032, 36.80131216085734280, 79.51042285023450518 ) ) ;
#5976 = ORIENTED_EDGE ( 'NONE', *, *, #17975, .T. ) ;
#5977 = ADVANCED_FACE ( 'NONE', ( #14191 ), #7712, .F. ) ;
#5978 = DIRECTION ( 'NONE',  ( 0.5813877811927012917, -0.8136266022444372803, -5.636455622144620416E-17 ) ) ;
#5979 = EDGE_CURVE ( 'NONE', #10089, #16685, #4507, .T. ) ;
#5980 = VERTEX_POINT ( 'NONE', #17287 ) ;
#5981 = CARTESIAN_POINT ( 'NONE',  ( -3.352688059453197589, 36.93499797900584980, 75.66110898724838307 ) ) ;
#5982 = EDGE_CURVE ( 'NONE', #5158, #2806, #11487, .T. ) ;
#5983 = DIRECTION ( 'NONE',  ( 1.540237394707284220E-16, 1.793354297423764243E-16, -1.000000000000000000 ) ) ;
#5984 = LINE ( 'NONE', #2998, #12699 ) ;
#5985 = PLANE ( 'NONE',  #19318 ) ;
#5986 = CARTESIAN_POINT ( 'NONE',  ( 9.125273767571991712, 43.16218137147968292, 75.00433879953099847 ) ) ;
#5987 = CARTESIAN_POINT ( 'NONE',  ( -5.810228987958474534, 37.89924280392040856, 75.80435357840198662 ) ) ;
#5988 = EDGE_CURVE ( 'NONE', #20868, #14733, #9420, .T. ) ;
#5989 = EDGE_CURVE ( 'NONE', #12039, #3841, #16115, .T. ) ;
#5990 = ORIENTED_EDGE ( 'NONE', *, *, #7931, .T. ) ;
#5991 = CARTESIAN_POINT ( 'NONE',  ( 4.597613975033692846, 52.09221767063174013, 78.17666347917207759 ) ) ;
#5992 = EDGE_CURVE ( 'NONE', #18376, #13415, #10823, .T. ) ;
#5993 = ORIENTED_EDGE ( 'NONE', *, *, #12352, .F. ) ;
#5994 = VECTOR ( 'NONE', #10101, 1000.000000000000000 ) ;
#5995 = DIRECTION ( 'NONE',  ( 6.308085367188358095E-15, 0.000000000000000000, 1.000000000000000000 ) ) ;
#5996 = CARTESIAN_POINT ( 'NONE',  ( 5.544968037009670780, 45.50804040601273925, 90.88308879953099506 ) ) ;
#5997 = CARTESIAN_POINT ( 'NONE',  ( -1.117719678584871090, 36.12782917792895176, 76.16022115247204738 ) ) ;
#5998 = ORIENTED_EDGE ( 'NONE', *, *, #7556, .F. ) ;
#5999 = CARTESIAN_POINT ( 'NONE',  ( -3.628867371436365730, 48.69222599884265179, 94.82933879782397923 ) ) ;
#6000 = LINE ( 'NONE', #12801, #12002 ) ;
#6001 = CARTESIAN_POINT ( 'NONE',  ( 0.5221537403065010796, 44.16218137147968292, 78.32492703482499508 ) ) ;
#6002 = CARTESIAN_POINT ( 'NONE',  ( 5.379940827581942919, 50.75970839669936652, 75.97198585835440099 ) ) ;
#6003 = VERTEX_POINT ( 'NONE', #14095 ) ;
#6004 = LINE ( 'NONE', #18987, #10892 ) ;
#6005 = CARTESIAN_POINT ( 'NONE',  ( 0.5886303428198357279, 52.96555932043412440, 78.93669174070734584 ) ) ;
#6006 = ORIENTED_EDGE ( 'NONE', *, *, #10629, .F. ) ;
#6007 = CARTESIAN_POINT ( 'NONE',  ( -4.537099264183359182, 37.70896829297682729, 78.53742703482498655 ) ) ;
#6008 = CARTESIAN_POINT ( 'NONE',  ( 5.295834872933118831, 46.52492710298120215, 95.05433879953093879 ) ) ;
#6009 = CARTESIAN_POINT ( 'NONE',  ( -5.616286711741428128, 44.43019146960381960, 91.39183879782399345 ) ) ;
#6010 = COLOUR_RGB ( '', 0.31764706, 0.68627451, 0.89019608) ;
#6011 = DIRECTION ( 'NONE',  ( -1.000000000000000000, 0.000000000000000000, 0.000000000000000000 ) ) ;
#6012 = ADVANCED_FACE ( 'NONE', ( #7918 ), #19397, .F. ) ;
#6013 = CARTESIAN_POINT ( 'NONE',  ( 8.849350546267242379, 41.31578948168061061, 75.97436175383765544 ) ) ;
#6014 = DIRECTION ( 'NONE',  ( -0.003146157466721092449, 0.009949137952083964009, 0.9999455566915655957 ) ) ;
#6015 = ORIENTED_EDGE ( 'NONE', *, *, #8319, .T. ) ;
#6016 = CARTESIAN_POINT ( 'NONE',  ( 1.645479938302748302, 52.89041620713354064, 76.88712749246440126 ) ) ;
#6017 = VERTEX_POINT ( 'NONE', #20670 ) ;
#6018 = CARTESIAN_POINT ( 'NONE',  ( 0.4007422551837632740, 52.36478753559008226, 79.54789450279270113 ) ) ;
#6019 = CARTESIAN_POINT ( 'NONE',  ( -0.9120904517194043937, 52.23579355909702571, 76.19475685965670664 ) ) ;
#6020 = CARTESIAN_POINT ( 'NONE',  ( -5.154188915835984375, 42.64120994080404614, 91.11746380123797451 ) ) ;
#6021 = VERTEX_POINT ( 'NONE', #14406 ) ;
#6022 = ORIENTED_EDGE ( 'NONE', *, *, #1689, .F. ) ;
#6023 = AXIS2_PLACEMENT_3D ( 'NONE', #8179, #3494, #5184 ) ;
#6024 = CARTESIAN_POINT ( 'NONE',  ( -3.138905401831777908, 36.85087662531303465, 75.96390267329995538 ) ) ;
#6025 = CARTESIAN_POINT ( 'NONE',  ( -7.100878668512206282, 41.13669111622050423, 76.88078815947486078 ) ) ;
#6026 = EDGE_LOOP ( 'NONE', ( #2453, #344, #7866, #3430, #4806 ) ) ;
#6027 = CARTESIAN_POINT ( 'NONE',  ( 2.029186242314200861, 35.35002428291939225, 76.16022115247204738 ) ) ;
#6028 = DIRECTION ( 'NONE',  ( -0.7071067811865515695, 0.7071067811865434649, 0.000000000000000000 ) ) ;
#6029 = CARTESIAN_POINT ( 'NONE',  ( 7.670764403146932864, 40.16467680216042169, 77.13595644658970230 ) ) ;
#6030 = ORIENTED_EDGE ( 'NONE', *, *, #13251, .T. ) ;
#6031 = CARTESIAN_POINT ( 'NONE',  ( -4.517072128342571880, 36.94403992325788977, 78.34992703482498655 ) ) ;
#6032 = CARTESIAN_POINT ( 'NONE',  ( -7.419646991370012934, 40.07141128159558008, 78.50801527011910252 ) ) ;
#6033 = CARTESIAN_POINT ( 'NONE',  ( -4.811608766808348037, 37.16160227343304712, 79.54845644658969661 ) ) ;
#6034 = CARTESIAN_POINT ( 'NONE',  ( 3.460444912181559474, 49.25145096859824889, 95.49246380123798872 ) ) ;
#6035 = FACE_OUTER_BOUND ( 'NONE', #8624, .T. ) ;
#6036 = CIRCLE ( 'NONE', #2298, 8.199999999999995737 ) ;
#6037 = CARTESIAN_POINT ( 'NONE',  ( 6.047224684482838342, 38.10257960454464410, 78.30195251056140648 ) ) ;
#6038 = VECTOR ( 'NONE', #18380, 1000.000000000000000 ) ;
#6039 = CARTESIAN_POINT ( 'NONE',  ( -1.477846259693499364, 49.81903562097207327, 83.21119304902337888 ) ) ;
#6040 = SURFACE_STYLE_FILL_AREA ( #10757 ) ;
#6041 = FACE_OUTER_BOUND ( 'NONE', #3732, .T. ) ;
#6042 = ORIENTED_EDGE ( 'NONE', *, *, #16509, .T. ) ;
#6043 = CARTESIAN_POINT ( 'NONE',  ( 8.616653853821931719, 45.47331367307960193, 79.47125056423675460 ) ) ;
#6044 = DIRECTION ( 'NONE',  ( -0.000000000000000000, 0.000000000000000000, -1.000000000000000000 ) ) ;
#6045 = CARTESIAN_POINT ( 'NONE',  ( 5.588830122182042004, 51.36004623135520575, 76.07177712439327877 ) ) ;
#6046 = CARTESIAN_POINT ( 'NONE',  ( -5.154188915835984375, 42.64120994080404614, 91.11746380123797451 ) ) ;
#6047 = EDGE_CURVE ( 'NONE', #9713, #5867, #6004, .T. ) ;
#6048 = AXIS2_PLACEMENT_3D ( 'NONE', #4462, #17350, #4562 ) ;
#6049 = CARTESIAN_POINT ( 'NONE',  ( -7.570386300417477621, 43.00511677435682145, 78.99227765976493743 ) ) ;
#6050 = CARTESIAN_POINT ( 'NONE',  ( 5.729336661111230633, 37.06727142202039715, 75.98270377909689444 ) ) ;
#6051 = ORIENTED_EDGE ( 'NONE', *, *, #12953, .F. ) ;
#6052 = DIRECTION ( 'NONE',  ( 0.007885122365275663500, 0.9999689119394085113, 1.805443505845543142E-16 ) ) ;
#6053 = FACE_OUTER_BOUND ( 'NONE', #4218, .T. ) ;
#6054 = CARTESIAN_POINT ( 'NONE',  ( 8.882424425600639495, 41.41491399621057923, 75.97389479739716478 ) ) ;
#6055 = DIRECTION ( 'NONE',  ( -0.000000000000000000, -0.000000000000000000, 1.000000000000000000 ) ) ;
#6056 = CARTESIAN_POINT ( 'NONE',  ( 5.254031822315176292, 50.85423277236746742, 78.06835901908682729 ) ) ;
#6057 = CARTESIAN_POINT ( 'NONE',  ( -4.205412028552263592, 50.86240891746721360, 78.93510015035742811 ) ) ;
#6058 = FACE_OUTER_BOUND ( 'NONE', #12392, .T. ) ;
#6059 = VECTOR ( 'NONE', #550, 1000.000000000000114 ) ;
#6060 = ORIENTED_EDGE ( 'NONE', *, *, #10030, .T. ) ;
#6061 = DIRECTION ( 'NONE',  ( -0.3165065846431827645, -0.9485903129789529098, 0.000000000000000000 ) ) ;
#6062 = CARTESIAN_POINT ( 'NONE',  ( 11.22215374030650281, 42.76218137147968434, 65.80574467885102763 ) ) ;
#6063 = EDGE_CURVE ( 'NONE', #8766, #12382, #15641, .T. ) ;
#6064 = CARTESIAN_POINT ( 'NONE',  ( -3.567022099613818664, 37.05453471803580356, 77.68963291717793140 ) ) ;
#6065 = VERTEX_POINT ( 'NONE', #14300 ) ;
#6066 = CARTESIAN_POINT ( 'NONE',  ( -0.1994209430448784792, 35.36759766960258844, 76.86610350541323555 ) ) ;
#6067 = CARTESIAN_POINT ( 'NONE',  ( 5.544968037009670780, 45.50804040601273925, 89.94558880294498238 ) ) ;
#6068 = ORIENTED_EDGE ( 'NONE', *, *, #16493, .F. ) ;
#6069 = CARTESIAN_POINT ( 'NONE',  ( 0.5221537403065064087, 48.16218137147969003, 85.55433879953100984 ) ) ;
#6070 = VECTOR ( 'NONE', #6698, 1000.000000000000114 ) ;
#6071 = CARTESIAN_POINT ( 'NONE',  ( -0.9338558694244919467, 52.21942839363907041, 76.50701133828320621 ) ) ;
#6072 = CARTESIAN_POINT ( 'NONE',  ( -4.453436368711327198, 50.68011839687689957, 76.44036821129557779 ) ) ;
#6073 = CARTESIAN_POINT ( 'NONE',  ( 11.22215374030650281, 42.76218137147968434, 73.80433879953100984 ) ) ;
#6074 = CARTESIAN_POINT ( 'NONE',  ( 0.8331116901989662482, 52.96370389921568034, 76.10706146582900544 ) ) ;
#6075 = CARTESIAN_POINT ( 'NONE',  ( -3.752375145463847428, 37.29320407110694191, 79.48068319027247242 ) ) ;
#6076 = ORIENTED_EDGE ( 'NONE', *, *, #14130, .T. ) ;
#6077 = CARTESIAN_POINT ( 'NONE',  ( 3.983393151002396326, 36.72848634532711287, 72.45433879953087342 ) ) ;
#6078 = EDGE_CURVE ( 'NONE', #2513, #1287, #20578, .T. ) ;
#6079 = ORIENTED_EDGE ( 'NONE', *, *, #2220, .F. ) ;
#6080 = CARTESIAN_POINT ( 'NONE',  ( 6.198496396448986090, 45.68315280215533392, 95.33621380123798872 ) ) ;
#6081 = CARTESIAN_POINT ( 'NONE',  ( -0.3080929418689875576, 37.85583172076933778, 94.94558880123797451 ) ) ;
#6082 = CARTESIAN_POINT ( 'NONE',  ( 2.722153740306517911, 49.95873206995546667, 56.15433879953099705 ) ) ;
#6083 = CARTESIAN_POINT ( 'NONE',  ( -4.506141062785093965, 37.68465281199856065, 77.90783589451615399 ) ) ;
#6084 = CARTESIAN_POINT ( 'NONE',  ( -3.349688636638950889, 52.21127678364309332, 76.69845644658968808 ) ) ;
#6085 = VECTOR ( 'NONE', #10114, 1000.000000000000000 ) ;
#6086 = VERTEX_POINT ( 'NONE', #16216 ) ;
#6087 = DIRECTION ( 'NONE',  ( 1.540237394707284220E-16, 1.793354297423764243E-16, -1.000000000000000000 ) ) ;
#6088 = ADVANCED_FACE ( 'NONE', ( #11336 ), #5785, .T. ) ;
#6089 = ADVANCED_FACE ( 'NONE', ( #6519 ), #11539, .T. ) ;
#6090 = ORIENTED_EDGE ( 'NONE', *, *, #11173, .F. ) ;
#6091 = CARTESIAN_POINT ( 'NONE',  ( -2.981657746618395333, 51.55448260090251722, 76.06019729239972094 ) ) ;
#6092 = CIRCLE ( 'NONE', #321, 0.9921021478795063464 ) ;
#6093 = B_SPLINE_CURVE_WITH_KNOTS ( 'NONE', 3,
 ( #2523, #4211, #15921, #7935, #1341, #2930, #17606, #12723, #1550, #12819, #9433, #9649, #19302, #19107, #14106, #9335 ),
 .UNSPECIFIED., .F., .F.,
 ( 4, 2, 2, 2, 2, 2, 2, 4 ),
 ( 0.000000000000000000, 0.0003384834742446624664, 0.0005077252113669950820, 0.0006769669484893277517, 0.0007615878170504936529, 0.0008462086856116595541, 0.001015450422733994284, 0.001353933896978663960 ),
 .UNSPECIFIED. ) ;
#6094 = CARTESIAN_POINT ( 'NONE',  ( 6.828503391016846891, 43.33193468930419101, 92.91433880123798872 ) ) ;
#6095 = CARTESIAN_POINT ( 'NONE',  ( 4.539372959821318609, 52.13523796247791608, 76.58963291717793709 ) ) ;
#6096 = ORIENTED_EDGE ( 'NONE', *, *, #2870, .F. ) ;
#6097 = VECTOR ( 'NONE', #15065, 1000.000000000000000 ) ;
#6098 = CARTESIAN_POINT ( 'NONE',  ( -5.381123819449237899, 50.75968757759591909, 79.33884456587460932 ) ) ;
#6099 = CARTESIAN_POINT ( 'NONE',  ( 5.220616844236031007, 45.87228208810806507, 93.73558879611698558 ) ) ;
#6100 = CARTESIAN_POINT ( 'NONE',  ( 5.566326199328858415, 51.37666897265353327, 76.21945306000542075 ) ) ;
#6101 = EDGE_CURVE ( 'NONE', #2938, #10515, #4915, .T. ) ;
#6102 = ORIENTED_EDGE ( 'NONE', *, *, #8352, .F. ) ;
#6103 = VECTOR ( 'NONE', #13886, 1000.000000000000000 ) ;
#6104 = CARTESIAN_POINT ( 'NONE',  ( -3.566428375817382257, 47.45690933515070498, 92.55433879953095300 ) ) ;
#6105 = AXIS2_PLACEMENT_3D ( 'NONE', #19827, #16652, #256 ) ;
#6106 = CARTESIAN_POINT ( 'NONE',  ( 1.352400422481993658, 50.46853102219002096, 90.72683880123797451 ) ) ;
#6107 = ORIENTED_EDGE ( 'NONE', *, *, #11342, .F. ) ;
#6108 = CARTESIAN_POINT ( 'NONE',  ( -2.073200253767597978, 36.38374080505226971, 75.45433879953088763 ) ) ;
#6109 = CYLINDRICAL_SURFACE ( 'NONE', #15293, 1.399999999999998579 ) ;
#6110 = AXIS2_PLACEMENT_3D ( 'NONE', #15286, #7072, #7297 ) ;
#6111 = CARTESIAN_POINT ( 'NONE',  ( 0.7901638384306286511, 50.30062182352762079, 92.32933879782399345 ) ) ;
#6112 = CIRCLE ( 'NONE', #20370, 4.000000000000000000 ) ;
#6113 = DIRECTION ( 'NONE',  ( 1.000000000000000000, -0.000000000000000000, -0.000000000000000000 ) ) ;
#6114 = CARTESIAN_POINT ( 'NONE',  ( 5.443310442819001338, 36.86288755851700927, 76.23948081211554495 ) ) ;
#6115 = CARTESIAN_POINT ( 'NONE',  ( -3.899663497332589213, 36.48798503826752437, 77.67016408458685817 ) ) ;
#6116 = ORIENTED_EDGE ( 'NONE', *, *, #16529, .T. ) ;
#6117 = CARTESIAN_POINT ( 'NONE',  ( 2.104760201255253538, 52.95427431201078150, 78.60861935269869605 ) ) ;
#6118 = AXIS2_PLACEMENT_3D ( 'NONE', #1814, #13188, #299 ) ;
#6119 = CARTESIAN_POINT ( 'NONE',  ( -3.462746425278574680, 37.07926700246258633, 77.72081520951157074 ) ) ;
#6120 = VECTOR ( 'NONE', #15872, 1000.000000000000000 ) ;
#6121 = ORIENTED_EDGE ( 'NONE', *, *, #11269, .F. ) ;
#6122 = CARTESIAN_POINT ( 'NONE',  ( 4.178421596892071044, 40.17206517740157778, 92.56371379953098710 ) ) ;
#6123 = ADVANCED_FACE ( 'NONE', ( #454 ), #15038, .T. ) ;
#6124 = CARTESIAN_POINT ( 'NONE',  ( 5.296683126097495808, 37.50502847857675448, 77.75931883872233641 ) ) ;
#6125 = CARTESIAN_POINT ( 'NONE',  ( -4.524181921268124462, 40.28999182795290324, 92.44558880123798872 ) ) ;
#6126 = B_SPLINE_SURFACE_WITH_KNOTS ( 'NONE', 3, 1, ( 
 ( #20076, #10105 ),
 ( #10534, #18497 ),
 ( #2008, #18181 ),
 ( #8505, #19963 ),
 ( #17004, #16898 ),
 ( #725, #19866 ),
 ( #10327, #3908 ),
 ( #8617, #5288 ),
 ( #11802, #10433 ),
 ( #7206, #18278 ),
 ( #833, #16695 ),
 ( #20184, #7319 ),
 ( #13808, #2118 ),
 ( #508, #6986 ),
 ( #8715, #13491 ) ),
 .UNSPECIFIED., .F., .F., .F.,
 ( 4, 1, 1, 1, 1, 1, 1, 1, 1, 1, 1, 1, 4 ),
 ( 2, 2 ),
 ( 0.000000000000000000, 0.1107947361882193060, 0.2116365373969002206, 0.3025951166517907298, 0.3827141919669941328, 0.4557983700405009997, 0.5187458605491411801, 0.5729830782426720281, 0.6198356358567430613, 0.7053145269299332387, 0.7944869293383459707, 0.8901174066118697770, 1.000000000000000000 ),
 ( 0.000000000000000000, 1.000000000000000000 ),
 .UNSPECIFIED. ) ;
#6127 = CARTESIAN_POINT ( 'NONE',  ( -0.8071739151948656987, 40.17810205696807913, 79.40903933791013003 ) ) ;
#6128 = EDGE_LOOP ( 'NONE', ( #19249, #5840, #6583, #16057 ) ) ;
#6129 = VERTEX_POINT ( 'NONE', #17807 ) ;
#6130 = VECTOR ( 'NONE', #11504, 1000.000000000000000 ) ;
#6131 = LINE ( 'NONE', #1562, #2994 ) ;
#6132 = CARTESIAN_POINT ( 'NONE',  ( -1.293305036878872549, 38.38734275159215059, 72.45433879953085921 ) ) ;
#6133 = ADVANCED_FACE ( 'NONE', ( #13125 ), #19600, .F. ) ;
#6134 = CARTESIAN_POINT ( 'NONE',  ( -5.389442353508429484, 49.84491604607124771, 76.26826950560264606 ) ) ;
#6135 = VERTEX_POINT ( 'NONE', #1754 ) ;
#6136 = CARTESIAN_POINT ( 'NONE',  ( 4.649988366678187823, 51.13951581206499952, 79.44143248960128290 ) ) ;
#6137 = CARTESIAN_POINT ( 'NONE',  ( 8.863132018971368709, 41.35709342965520818, 77.52392363563762956 ) ) ;
#6138 = CARTESIAN_POINT ( 'NONE',  ( -4.176309363623029292, 42.45208065485131499, 90.92308879953097289 ) ) ;
#6139 = EDGE_CURVE ( 'NONE', #11984, #11711, #18016, .T. ) ;
#6140 = VERTEX_POINT ( 'NONE', #1855 ) ;
#6141 = CARTESIAN_POINT ( 'NONE',  ( 5.700162184304335966, 50.52331579763416869, 75.37176668953071612 ) ) ;
#6142 = CARTESIAN_POINT ( 'NONE',  ( -6.751500244480902246, 40.44442896114340158, 79.01214282451080351 ) ) ;
#6143 = CARTESIAN_POINT ( 'NONE',  ( 6.403592332820982946, 38.44823507962264841, 76.00831143408265689 ) ) ;
#6144 = CARTESIAN_POINT ( 'NONE',  ( 3.122075258343615545, 38.59543968120053847, 90.21201841395856036 ) ) ;
#6145 =( LENGTH_UNIT ( ) NAMED_UNIT ( * ) SI_UNIT ( .MILLI., .METRE. ) );
#6146 = CARTESIAN_POINT ( 'NONE',  ( 6.450247442662826458, 38.49669771550791353, 77.26022115247205591 ) ) ;
#6147 = DIRECTION ( 'NONE',  ( -0.000000000000000000, -2.168404344970984413E-15, -1.000000000000000000 ) ) ;
#6148 = CARTESIAN_POINT ( 'NONE',  ( -1.477846259693492037, 50.16218137147969713, 69.55433879953100984 ) ) ;
#6149 = CARTESIAN_POINT ( 'NONE',  ( -0.2726345245567728393, 52.97463310108326340, 79.40856224512604911 ) ) ;
#6150 = ORIENTED_EDGE ( 'NONE', *, *, #1300, .F. ) ;
#6151 = CARTESIAN_POINT ( 'NONE',  ( -1.477846259693491149, 47.62628298661744708, 50.55433879953100273 ) ) ;
#6152 = CARTESIAN_POINT ( 'NONE',  ( -1.477846259693493813, 50.16218137147969713, 74.55433879953100984 ) ) ;
#6153 = CARTESIAN_POINT ( 'NONE',  ( 5.570264759168902735, 51.37375971715457013, 76.17377400622436312 ) ) ;
#6154 = CIRCLE ( 'NONE', #18736, 3.999999999999996447 ) ;
#6155 = ORIENTED_EDGE ( 'NONE', *, *, #13213, .T. ) ;
#6156 = EDGE_CURVE ( 'NONE', #4005, #7893, #8339, .T. ) ;
#6157 = VERTEX_POINT ( 'NONE', #5448 ) ;
#6158 = DIRECTION ( 'NONE',  ( -0.000000000000000000, -0.000000000000000000, 1.000000000000000000 ) ) ;
#6159 = CARTESIAN_POINT ( 'NONE',  ( -5.531051774427890422, 44.10426199826898142, 72.45433879953085921 ) ) ;
#6160 = CARTESIAN_POINT ( 'NONE',  ( -1.477846259693493813, 49.76218137147969856, 77.55433879953099563 ) ) ;
#6161 = LINE ( 'NONE', #4559, #17121 ) ;
#6162 = CARTESIAN_POINT ( 'NONE',  ( 8.876519138579782364, 41.39721547638464472, 77.52397343602532942 ) ) ;
#6163 = VECTOR ( 'NONE', #6271, 1000.000000000000114 ) ;
#6164 = CARTESIAN_POINT ( 'NONE',  ( 9.353599821682333726, 42.82705654907719151, 77.11956464767864361 ) ) ;
#6165 = PLANE ( 'NONE',  #19638 ) ;
#6166 = CARTESIAN_POINT ( 'NONE',  ( 5.205086686352852432, 50.89348831148397778, 76.20630380245266622 ) ) ;
#6167 = VECTOR ( 'NONE', #3819, 1000.000000000000000 ) ;
#6168 = CARTESIAN_POINT ( 'NONE',  ( 30.43948732994509143, 43.16218137147969003, 76.90433879953101837 ) ) ;
#6169 = EDGE_CURVE ( 'NONE', #11401, #11113, #10199, .T. ) ;
#6170 = CARTESIAN_POINT ( 'NONE',  ( 10.77494014480653917, 42.76218137147968434, 61.80715055817104542 ) ) ;
#6171 = CARTESIAN_POINT ( 'NONE',  ( 3.357643116058060873, 37.76218137147968434, 95.05433879953096721 ) ) ;
#6172 = ORIENTED_EDGE ( 'NONE', *, *, #2896, .T. ) ;
#6173 = AXIS2_PLACEMENT_3D ( 'NONE', #13898, #20382, #15613 ) ;
#6174 = LINE ( 'NONE', #17358, #10222 ) ;
#6175 = CARTESIAN_POINT ( 'NONE',  ( 5.025485839985549319, 41.56218137147963887, 89.78933880294498238 ) ) ;
#6176 = ORIENTED_EDGE ( 'NONE', *, *, #12464, .F. ) ;
#6177 = CARTESIAN_POINT ( 'NONE',  ( 5.901490163600553451, 51.12909685347405286, 78.67852979887695142 ) ) ;
#6178 = CARTESIAN_POINT ( 'NONE',  ( -0.9427404655910675002, 52.21949845194497897, 76.89011419028814487 ) ) ;
#6179 = CARTESIAN_POINT ( 'NONE',  ( 8.425866390803962602, 42.00143579340615929, 78.13577067582016866 ) ) ;
#6180 = CARTESIAN_POINT ( 'NONE',  ( -4.453436368711328974, 50.68011839687689957, 78.45066232894264147 ) ) ;
#6181 = CARTESIAN_POINT ( 'NONE',  ( 0.5705748789227172990, 52.35433120667131135, 75.97198585835440099 ) ) ;
#6182 = CARTESIAN_POINT ( 'NONE',  ( 1.618771744999037754, 49.47142490715005181, 92.45433879953100131 ) ) ;
#6183 = EDGE_LOOP ( 'NONE', ( #10909, #3666, #2404, #4188 ) ) ;
#6184 = CARTESIAN_POINT ( 'NONE',  ( 8.292349522058055200, 41.56647775562769453, 75.97198585835440099 ) ) ;
#6185 = ORIENTED_EDGE ( 'NONE', *, *, #6387, .T. ) ;
#6186 = CARTESIAN_POINT ( 'NONE',  ( -0.3080929418689875576, 37.85583172076933778, 93.69558880123800293 ) ) ;
#6187 = EDGE_CURVE ( 'NONE', #10035, #8755, #4174, .T. ) ;
#6188 = CARTESIAN_POINT ( 'NONE',  ( 6.457023732898393042, 39.40536329938229443, 72.45432679953087529 ) ) ;
#6189 = CARTESIAN_POINT ( 'NONE',  ( 0.3292270019246527069, 52.35991533748182292, 76.18796821092257687 ) ) ;
#6190 = AXIS2_PLACEMENT_3D ( 'NONE', #9462, #14345, #10654 ) ;
#6191 = CARTESIAN_POINT ( 'NONE',  ( 5.824901997307729395, 37.13555891239614226, 76.06531707679772580 ) ) ;
#6192 = DIRECTION ( 'NONE',  ( -1.110223024625156540E-16, -1.000000000000000000, -5.922860397471808077E-17 ) ) ;
#6193 = AXIS2_PLACEMENT_3D ( 'NONE', #16844, #2263, #7146 ) ;
#6194 = ORIENTED_EDGE ( 'NONE', *, *, #5660, .T. ) ;
#6195 = CARTESIAN_POINT ( 'NONE',  ( 4.715683878568929011, 52.00500418903608590, 77.90619853385557292 ) ) ;
#6196 = VERTEX_POINT ( 'NONE', #7150 ) ;
#6197 = DIRECTION ( 'NONE',  ( -0.5941461771851691553, -0.8043570849667760481, -2.357623395011396791E-16 ) ) ;
#6198 = EDGE_CURVE ( 'NONE', #5069, #1854, #15362, .T. ) ;
#6199 = CARTESIAN_POINT ( 'NONE',  ( -4.567115856812060670, 47.10047254335474065, 95.96121380123798872 ) ) ;
#6200 = CARTESIAN_POINT ( 'NONE',  ( 4.661142417382979630, 52.04529176935007939, 75.82370277575662953 ) ) ;
#6201 = ORIENTED_EDGE ( 'NONE', *, *, #15051, .F. ) ;
#6202 = CARTESIAN_POINT ( 'NONE',  ( -5.400510509167274265, 49.82588755935344693, 78.31711373209397209 ) ) ;
#6203 = DIRECTION ( 'NONE',  ( 1.540237394707284220E-16, 1.793354297423764243E-16, -1.000000000000000000 ) ) ;
#6204 = EDGE_LOOP ( 'NONE', ( #3344, #20450, #20888, #6267 ) ) ;
#6205 = AXIS2_PLACEMENT_3D ( 'NONE', #798, #20247, #5676 ) ;
#6207 = FACE_OUTER_BOUND ( 'NONE', #11570, .T. ) ;
#6206 = B_SPLINE_CURVE_WITH_KNOTS ( 'NONE', 3,
 ( #2770, #19241, #10978, #17343, #7869, #7764, #14358, #14242, #9161, #15653, #12760, #12355 ),
 .UNSPECIFIED., .F., .F.,
 ( 4, 2, 2, 2, 2, 4 ),
 ( 0.000000000000000000, 0.0001655740708910906161, 0.0003311481417821812321, 0.0004139351772277070516, 0.0004967222126732328711, 0.0006622962835642647777 ),
 .UNSPECIFIED. ) ;
#6208 = CARTESIAN_POINT ( 'NONE',  ( -4.061474658916792713, 50.95574512005268275, 78.82303764823565473 ) ) ;
#6209 = FACE_BOUND ( 'NONE', #7670, .T. ) ;
#6210 = VERTEX_POINT ( 'NONE', #2581 ) ;
#6211 = CARTESIAN_POINT ( 'NONE',  ( -4.615702297814525679, 45.70854999956944198, 92.55433879953100984 ) ) ;
#6212 = CARTESIAN_POINT ( 'NONE',  ( -5.154188915835984375, 42.64120994080404614, 92.36746380123797451 ) ) ;
#6213 = ORIENTED_EDGE ( 'NONE', *, *, #2689, .T. ) ;
#6214 = CARTESIAN_POINT ( 'NONE',  ( 4.140412088821458170, 51.51591928153320765, 78.46169174070733732 ) ) ;
#6215 = CARTESIAN_POINT ( 'NONE',  ( 2.122153740306507164, 47.82824192744436687, 85.55433879953100984 ) ) ;
#6216 = CARTESIAN_POINT ( 'NONE',  ( 0.8503282811412331554, 52.95606000782370870, 78.52566232894263010 ) ) ;
#6217 = CARTESIAN_POINT ( 'NONE',  ( 3.394636754364005693, 39.16678693318392135, 95.56538169964434815 ) ) ;
#6218 = CARTESIAN_POINT ( 'NONE',  ( 5.497686461428984650, 36.90174267058258550, 76.03636210503219672 ) ) ;
#6219 = CARTESIAN_POINT ( 'NONE',  ( -3.944959226007137776, 38.51060946023304865, 78.18375056423674607 ) ) ;
#6220 = VECTOR ( 'NONE', #10925, 1000.000000000000227 ) ;
#6221 = CARTESIAN_POINT ( 'NONE',  ( -3.607485548685021914, 36.27216495724724155, 77.44024473021482891 ) ) ;
#6222 = ORIENTED_EDGE ( 'NONE', *, *, #13956, .T. ) ;
#6223 = CARTESIAN_POINT ( 'NONE',  ( 2.112089635657790954, 52.20154156089598274, 78.36218633565054859 ) ) ;
#6224 = ORIENTED_EDGE ( 'NONE', *, *, #12185, .T. ) ;
#6225 = LINE ( 'NONE', #16030, #9861 ) ;
#6226 = LINE ( 'NONE', #12727, #15370 ) ;
#6227 = CARTESIAN_POINT ( 'NONE',  ( -4.498303996637021740, 46.81144376258747997, 95.05433879953096721 ) ) ;
#6228 = ORIENTED_EDGE ( 'NONE', *, *, #8018, .T. ) ;
#6229 = CARTESIAN_POINT ( 'NONE',  ( -1.219056181836354558, 49.77488197367695477, 93.31237966814926210 ) ) ;
#6230 = ORIENTED_EDGE ( 'NONE', *, *, #10160, .T. ) ;
#6231 = CARTESIAN_POINT ( 'NONE',  ( -4.169456222845758120, 37.61210300367680048, 75.36135576041903050 ) ) ;
#6232 = LINE ( 'NONE', #8048, #669 ) ;
#6233 = CARTESIAN_POINT ( 'NONE',  ( -7.210177143685434942, 41.42808673320669755, 76.51871785122798997 ) ) ;
#6234 = ORIENTED_EDGE ( 'NONE', *, *, #20564, .F. ) ;
#6235 = CARTESIAN_POINT ( 'NONE',  ( -4.517625420443600603, 36.94444861784495515, 76.85096240152589075 ) ) ;
#6236 = CARTESIAN_POINT ( 'NONE',  ( 5.740585635973905809, 51.24795054640212300, 75.97198585835440099 ) ) ;
#6237 = CARTESIAN_POINT ( 'NONE',  ( -5.616286711741428128, 44.43019146960381960, 91.23558879782397923 ) ) ;
#6238 = CIRCLE ( 'NONE', #20161, 4.000000000000003553 ) ;
#6239 = VERTEX_POINT ( 'NONE', #5336 ) ;
#6240 = FACE_OUTER_BOUND ( 'NONE', #1314, .T. ) ;
#6241 = CARTESIAN_POINT ( 'NONE',  ( 5.748274343403733333, 51.24227120794373747, 77.94845644658968808 ) ) ;
#6242 = CARTESIAN_POINT ( 'NONE',  ( 5.925147347628167971, 37.99321178357424600, 75.45609877704765722 ) ) ;
#6243 = CARTESIAN_POINT ( 'NONE',  ( 3.460444912181559474, 49.25145096859824889, 90.64871380123798872 ) ) ;
#6244 = ADVANCED_FACE ( 'NONE', ( #18544, #17161 ), #3855, .T. ) ;
#6245 = EDGE_CURVE ( 'NONE', #12496, #12950, #15545, .T. ) ;
#6246 = CARTESIAN_POINT ( 'NONE',  ( -4.652687709939232086, 51.28020135170361016, 75.36022115247205022 ) ) ;
#6247 = CARTESIAN_POINT ( 'NONE',  ( 0.9516664821082820858, 52.34032181963752350, 76.77464780632124075 ) ) ;
#6248 = ADVANCED_FACE ( 'NONE', ( #13755 ), #5772, .T. ) ;
#6249 = DIRECTION ( 'NONE',  ( -1.779391786395883536E-16, -5.922860397471806844E-17, 1.000000000000000000 ) ) ;
#6250 = EDGE_CURVE ( 'NONE', #14881, #12080, #8493, .T. ) ;
#6251 = CARTESIAN_POINT ( 'NONE',  ( -0.5458045384150788104, 52.97678714703417313, 79.25925238658010130 ) ) ;
#6252 = DIRECTION ( 'NONE',  ( -1.193617070626243484E-16, -1.000000000000000000, -0.000000000000000000 ) ) ;
#6253 = DIRECTION ( 'NONE',  ( -1.110223024625156540E-16, -1.000000000000000000, -5.922860397471808077E-17 ) ) ;
#6254 = CARTESIAN_POINT ( 'NONE',  ( 8.390051116449676272, 39.93923995310483832, 78.49952087821802138 ) ) ;
#6255 = CARTESIAN_POINT ( 'NONE',  ( 8.787829143201870252, 41.13140593384865440, 76.40801527011910821 ) ) ;
#6256 = EDGE_CURVE ( 'NONE', #8809, #13618, #10481, .T. ) ;
#6257 = ORIENTED_EDGE ( 'NONE', *, *, #12803, .T. ) ;
#6258 = CARTESIAN_POINT ( 'NONE',  ( -4.511982275096481310, 37.68935279624734846, 78.82711781305037846 ) ) ;
#6259 = CARTESIAN_POINT ( 'NONE',  ( 29.63948732994508006, 45.16218137147969003, 76.90433879953101837 ) ) ;
#6260 = DIRECTION ( 'NONE',  ( 1.000000000000000000, -1.193617070626243237E-16, 5.626130192357177659E-16 ) ) ;
#6261 = DIRECTION ( 'NONE',  ( 1.000000000000000000, 1.402518428993831676E-16, -4.865963288531424989E-32 ) ) ;
#6262 = CARTESIAN_POINT ( 'NONE',  ( 8.933414522996312002, 41.56773455285687646, 77.44430071719698105 ) ) ;
#6263 = CARTESIAN_POINT ( 'NONE',  ( 6.961260622506120654, 50.34628710563859499, 76.69700829373513784 ) ) ;
#6264 = PLANE ( 'NONE',  #9800 ) ;
#6265 = CARTESIAN_POINT ( 'NONE',  ( 6.960985561621730433, 50.34649028203376275, 76.51259071708746262 ) ) ;
#6266 =( REPRESENTATION_RELATIONSHIP ('NONE','NONE', #11365, #209 ) REPRESENTATION_RELATIONSHIP_WITH_TRANSFORMATION ( #20260 )SHAPE_REPRESENTATION_RELATIONSHIP( ) );
#6267 = ORIENTED_EDGE ( 'NONE', *, *, #18869, .F. ) ;
#6268 = EDGE_CURVE ( 'NONE', #11304, #17122, #879, .T. ) ;
#6269 = CARTESIAN_POINT ( 'NONE',  ( -4.811608766808351589, 37.16160227343304712, 79.54845644658969661 ) ) ;
#6270 = DIRECTION ( 'NONE',  ( 0.3165065846431827645, 0.9485903129789529098, 0.000000000000000000 ) ) ;
#6271 = DIRECTION ( 'NONE',  ( -0.9485903129789527988, 0.3165065846431829311, -8.934458285744989980E-17 ) ) ;
#6272 = ORIENTED_EDGE ( 'NONE', *, *, #8197, .F. ) ;
#6273 = DIRECTION ( 'NONE',  ( -4.344610079045915326E-32, -6.093395702654244599E-48, -1.000000000000000000 ) ) ;
#6274 = CARTESIAN_POINT ( 'NONE',  ( 4.613683985508550300, 40.84891963687440608, 89.75946567728124137 ) ) ;
#6275 = ORIENTED_EDGE ( 'NONE', *, *, #19507, .T. ) ;
#6276 = CARTESIAN_POINT ( 'NONE',  ( -0.6425283709582511049, 52.97632458963546753, 75.74123345422913189 ) ) ;
#6277 = B_SPLINE_CURVE_WITH_KNOTS ( 'NONE', 3,
 ( #14773, #3188, #7977, #9693, #14462, #17967, #9789, #12863, #8394, #8181, #17860, #16171, #19343, #19658, #1594, #14568 ),
 .UNSPECIFIED., .F., .F.,
 ( 4, 2, 2, 2, 2, 2, 2, 4 ),
 ( 8.673617379884035472E-19, 0.0005211411850466844947, 0.0007817117775700237062, 0.001042282370093363135, 0.001302852962616702238, 0.001563423555140041558, 0.001823994147663380878, 0.002084564740186720198 ),
 .UNSPECIFIED. ) ;
#6278 = CARTESIAN_POINT ( 'NONE',  ( 8.439922054675561114, 42.04356150970401984, 78.13669174070733447 ) ) ;
#6279 = CARTESIAN_POINT ( 'NONE',  ( 6.046986631774924348, 37.29425246114896453, 78.37121987722640881 ) ) ;
#6280 = CARTESIAN_POINT ( 'NONE',  ( -5.530828587017968978, 50.65271403173267117, 79.22855648223701053 ) ) ;
#6281 = CARTESIAN_POINT ( 'NONE',  ( 4.193944868301254125, 47.85951822794249466, 92.45433879953095868 ) ) ;
#6282 = ORIENTED_EDGE ( 'NONE', *, *, #13239, .F. ) ;
#6283 = CARTESIAN_POINT ( 'NONE',  ( -1.219503646467431590, 49.90383875825363447, 61.41268141275705972 ) ) ;
#6284 = ORIENTED_EDGE ( 'NONE', *, *, #6361, .F. ) ;
#6285 = LINE ( 'NONE', #14383, #16255 ) ;
#6286 = DIRECTION ( 'NONE',  ( 1.000000000000000000, 0.000000000000000000, 0.000000000000000000 ) ) ;
#6287 = DIRECTION ( 'NONE',  ( 0.9485903129789527988, -0.3165065846431829311, 8.934458285744989980E-17 ) ) ;
#6288 = LINE ( 'NONE', #9818, #15088 ) ;
#6289 = CARTESIAN_POINT ( 'NONE',  ( -4.209923912819721892, 38.70632820095286775, 77.33669174070733732 ) ) ;
#6290 = B_SPLINE_SURFACE_WITH_KNOTS ( 'NONE', 3, 1, ( 
 ( #4768, #3288 ),
 ( #13189, #19559 ),
 ( #11606, #4979 ),
 ( #9907, #19662 ),
 ( #18082, #1907 ),
 ( #8399, #4431 ),
 ( #10944, #7945 ),
 ( #2939, #17311 ),
 ( #6024, #1146 ),
 ( #9445, #12734 ),
 ( #12831, #4317 ),
 ( #4529, #1459 ),
 ( #11046, #15931 ),
 ( #18905, #15728 ),
 ( #20804, #2737 ),
 ( #19311, #4626 ),
 ( #19211, #1351 ),
 ( #11147, #4727 ),
 ( #7633, #14428 ),
 ( #17416, #10843 ),
 ( #7843, #14325 ),
 ( #9345, #2842 ),
 ( #7734, #15830 ),
 ( #1241, #20898 ),
 ( #6231, #9239 ),
 ( #12523, #14114 ),
 ( #17615, #3047 ) ),
 .UNSPECIFIED., .F., .F., .F.,
 ( 4, 1, 1, 1, 1, 1, 1, 1, 1, 1, 1, 1, 1, 1, 1, 1, 1, 1, 1, 1, 1, 1, 1, 1, 4 ),
 ( 2, 2 ),
 ( 0.000000000000000000, 0.04981064803454772483, 0.09714544705284619552, 0.1414600528990057893, 0.1834992459999073566, 0.2227657660311612720, 0.2600403684493295953, 0.2949019026928859644, 0.3281718573768891978, 0.3602550803352915776, 0.3926260793274650163, 0.4253773651182169435, 0.4592860034499685606, 0.4939555262694102500, 0.5299277977440765008, 0.5677681756169172811, 0.6073809588441169138, 0.6486765994917140787, 0.6919144726687150859, 0.7374495574558619371, 0.7851062196494249523, 0.8349986418379958808, 0.8875444209637680659, 0.9425288195084158271, 1.000000000000000000 ),
 ( 0.000000000000000000, 1.000000000000000000 ),
 .UNSPECIFIED. ) ;
#6291 = ORIENTED_EDGE ( 'NONE', *, *, #3722, .F. ) ;
#6292 = CARTESIAN_POINT ( 'NONE',  ( 4.837856207073459203, 51.91476041137136832, 77.79664654212120922 ) ) ;
#6293 =( BOUNDED_CURVE ( )  B_SPLINE_CURVE ( 3, ( #7541, #2542, #15946, #6039 ),
 .UNSPECIFIED., .F., .T. ) 
 B_SPLINE_CURVE_WITH_KNOTS ( ( 4, 4 ),
 ( 2.801755744135677961, 3.481429563043919373 ),
 .UNSPECIFIED. ) 
 CURVE ( )  GEOMETRIC_REPRESENTATION_ITEM ( )  RATIONAL_B_SPLINE_CURVE ( ( 1.000000000000000000, 0.9618726943880424596, 0.9618726943880424596, 1.000000000000000000 ) ) 
 REPRESENTATION_ITEM ( '' )  );
#6294 = VERTEX_POINT ( 'NONE', #2165 ) ;
#6295 = LINE ( 'NONE', #12489, #12568 ) ;
#6296 = CARTESIAN_POINT ( 'NONE',  ( 6.102441102155617969, 43.42752260303680600, 90.80496379953099506 ) ) ;
#6297 = CARTESIAN_POINT ( 'NONE',  ( -7.826013883771545387, 41.35585863650159411, 78.20300316143082853 ) ) ;
#6298 = VERTEX_POINT ( 'NONE', #7364 ) ;
#6299 = ADVANCED_FACE ( 'NONE', ( #12166 ), #20224, .T. ) ;
#6300 = CARTESIAN_POINT ( 'NONE',  ( -5.761564881245698544, 50.48783832367244884, 78.87652712212219797 ) ) ;
#6301 = CARTESIAN_POINT ( 'NONE',  ( -1.477846259693506914, 47.62628298661743997, 85.15433879953098995 ) ) ;
#6302 = CARTESIAN_POINT ( 'NONE',  ( -4.539440361571186244, 36.96056243609646685, 78.81995494622690046 ) ) ;
#6303 = CARTESIAN_POINT ( 'NONE',  ( 5.259329269783745708, 50.84879929591499348, 76.01203914421944319 ) ) ;
#6304 = CARTESIAN_POINT ( 'NONE',  ( 4.199109002476567376, 47.83913663364971569, 93.48786078214052964 ) ) ;
#6305 = ORIENTED_EDGE ( 'NONE', *, *, #6256, .T. ) ;
#6306 = CARTESIAN_POINT ( 'NONE',  ( -4.898402303810498459, 43.01822212045506433, 92.55433879953096721 ) ) ;
#6307 = CARTESIAN_POINT ( 'NONE',  ( 0.7959481941832846630, 52.35792193448483545, 76.79590682236855059 ) ) ;
#6308 = ORIENTED_EDGE ( 'NONE', *, *, #10579, .F. ) ;
#6309 = CARTESIAN_POINT ( 'NONE',  ( -0.6433819530550480836, 49.43133198673770323, 95.05433879953093879 ) ) ;
#6310 = DIRECTION ( 'NONE',  ( 0.3165065846431827645, 0.9485903129789529098, 0.000000000000000000 ) ) ;
#6311 = CARTESIAN_POINT ( 'NONE',  ( -5.400724308821385655, 49.82590620323193065, 76.54939005541714891 ) ) ;
#6312 = CARTESIAN_POINT ( 'NONE',  ( -5.616286711741429905, 44.43019146960381960, 92.64183879782400766 ) ) ;
#6313 = CARTESIAN_POINT ( 'NONE',  ( 31.07218010054375412, 42.76218137147968434, 70.80574467885102763 ) ) ;
#6314 = DIRECTION ( 'NONE',  ( 1.110223024625156540E-16, 1.000000000000000000, 5.922860397471808077E-17 ) ) ;
#6315 = AXIS2_PLACEMENT_3D ( 'NONE', #7009, #18517, #15010 ) ;
#6316 = CARTESIAN_POINT ( 'NONE',  ( -3.115445724116070902, 36.83354790639791077, 77.32142682847380399 ) ) ;
#6317 = ORIENTED_EDGE ( 'NONE', *, *, #3709, .T. ) ;
#6318 = CARTESIAN_POINT ( 'NONE',  ( 2.098825451632840178, 52.20164615386168805, 78.60861935269869605 ) ) ;
#6319 = CARTESIAN_POINT ( 'NONE',  ( -3.799298760401091268, 51.89000185047994052, 75.54713691134779197 ) ) ;
#6320 = ORIENTED_EDGE ( 'NONE', *, *, #13177, .F. ) ;
#6321 = LINE ( 'NONE', #12934, #18000 ) ;
#6322 = CARTESIAN_POINT ( 'NONE',  ( 30.43948732994507722, 36.35905713404685002, 74.70433879953098710 ) ) ;
#6323 = CARTESIAN_POINT ( 'NONE',  ( 9.353817388681445522, 42.82770861117572281, 78.41904468188381827 ) ) ;
#6324 = CARTESIAN_POINT ( 'NONE',  ( -2.932686190032669948, 51.59885408774670879, 76.34467759591066738 ) ) ;
#6325 = ORIENTED_EDGE ( 'NONE', *, *, #3217, .T. ) ;
#6326 = FACE_OUTER_BOUND ( 'NONE', #17289, .T. ) ;
#6327 = VERTEX_POINT ( 'NONE', #3744 ) ;
#6328 = EDGE_CURVE ( 'NONE', #16577, #16572, #8664, .T. ) ;
#6329 = CARTESIAN_POINT ( 'NONE',  ( -7.949137504989498559, 41.77948864320536160, 78.50654468188380974 ) ) ;
#6330 = CARTESIAN_POINT ( 'NONE',  ( 8.377992009893507230, 41.81147811158319172, 78.64980314354953350 ) ) ;
#6331 = DIRECTION ( 'NONE',  ( -0.5813877811927012917, 0.8136266022444372803, 5.636455622144620416E-17 ) ) ;
#6332 = ORIENTED_EDGE ( 'NONE', *, *, #13276, .F. ) ;
#6333 = CARTESIAN_POINT ( 'NONE',  ( -4.359867457993620299, 37.60268028463676870, 77.29630340639747033 ) ) ;
#6334 = DIRECTION ( 'NONE',  ( -0.3165065846431825980, -0.9485903129789530208, 0.000000000000000000 ) ) ;
#6335 = CARTESIAN_POINT ( 'NONE',  ( 2.232254456934871456, 39.46371826755015633, 93.73558879953097289 ) ) ;
#6336 = AXIS2_PLACEMENT_3D ( 'NONE', #8341, #16119, #3024 ) ;
#6337 = VERTEX_POINT ( 'NONE', #558 ) ;
#6338 = CARTESIAN_POINT ( 'NONE',  ( -4.699529792962120034, 51.24672971417357559, 75.98997946140892168 ) ) ;
#6339 = CARTESIAN_POINT ( 'NONE',  ( 25.63948732994507651, 45.16218137147968292, 74.70433879953100131 ) ) ;
#6340 = DIRECTION ( 'NONE',  ( 1.000000000000000000, -1.110223024625156417E-16, -1.111814006898795283E-16 ) ) ;
#6341 = CARTESIAN_POINT ( 'NONE',  ( -5.784195910403845176, 44.99242805365518194, 93.53933880123797451 ) ) ;
#6342 = CARTESIAN_POINT ( 'NONE',  ( 5.611423337425062385, 41.22389019960463230, 92.67996380123798872 ) ) ;
#6343 = EDGE_CURVE ( 'NONE', #5798, #5122, #7040, .T. ) ;
#6344 = CARTESIAN_POINT ( 'NONE',  ( 8.230299787179362170, 47.07948288808702841, 79.45405409817819020 ) ) ;
#6345 = EDGE_CURVE ( 'NONE', #3158, #20516, #4128, .T. ) ;
#6346 = CARTESIAN_POINT ( 'NONE',  ( 0.3327597288346153537, 52.96805686913342015, 77.10139762306027933 ) ) ;
#6347 = FACE_OUTER_BOUND ( 'NONE', #12294, .T. ) ;
#6348 = CARTESIAN_POINT ( 'NONE',  ( -0.9437865455955903871, 52.21748465046702137, 77.77566232894263010 ) ) ;
#6349 = VECTOR ( 'NONE', #13830, 1000.000000000000000 ) ;
#6350 = ORIENTED_EDGE ( 'NONE', *, *, #13739, .T. ) ;
#6351 = CARTESIAN_POINT ( 'NONE',  ( -4.158995335318336650, 37.42966003176047707, 76.41545151846887052 ) ) ;
#6352 = CARTESIAN_POINT ( 'NONE',  ( 2.722153740306497927, 50.36218137147968577, 54.55433879953098852 ) ) ;
#6353 = ADVANCED_FACE ( 'NONE', ( #14072 ), #9502, .F. ) ;
#6354 = CARTESIAN_POINT ( 'NONE',  ( 0.8402845321420674418, 52.35600907897080702, 76.16933144905489428 ) ) ;
#6355 = CARTESIAN_POINT ( 'NONE',  ( 0.7444978820518556306, 52.95993232485279378, 79.54697877576636245 ) ) ;
#6356 = EDGE_CURVE ( 'NONE', #8103, #14909, #12478, .T. ) ;
#6357 = ORIENTED_EDGE ( 'NONE', *, *, #19506, .F. ) ;
#6358 = VECTOR ( 'NONE', #18934, 1000.000000000000000 ) ;
#6359 = CARTESIAN_POINT ( 'NONE',  ( 4.199109002476567376, 47.83913663364971569, 93.80036078555450274 ) ) ;
#6360 = DIRECTION ( 'NONE',  ( 1.000000000000000000, 0.000000000000000000, 0.000000000000000000 ) ) ;
#6361 = EDGE_CURVE ( 'NONE', #15505, #13342, #2900, .T. ) ;
#6362 = CARTESIAN_POINT ( 'NONE',  ( -4.895222749246782357, 37.22336455408366618, 78.59503622499421738 ) ) ;
#6363 = CARTESIAN_POINT ( 'NONE',  ( 5.722153740306500147, 44.16218137147969003, 77.84651775085080772 ) ) ;
#6364 = CARTESIAN_POINT ( 'NONE',  ( 5.239838662427071192, 50.86471668784145805, 78.21422674182478829 ) ) ;
#6365 = VECTOR ( 'NONE', #14805, 1000.000000000000114 ) ;
#6366 = CARTESIAN_POINT ( 'NONE',  ( 32.72215374030650281, 44.16218137147968292, 93.55433879953098142 ) ) ;
#6367 = CARTESIAN_POINT ( 'NONE',  ( 6.888069329080921399, 50.40035056576664374, 77.33077842133744184 ) ) ;
#6368 = FACE_OUTER_BOUND ( 'NONE', #20109, .T. ) ;
#6369 = DIRECTION ( 'NONE',  ( -1.402518428993831676E-16, 1.000000000000000000, 0.000000000000000000 ) ) ;
#6370 = CARTESIAN_POINT ( 'NONE',  ( 8.788011242024285963, 41.13195169557157271, 78.55826321071354812 ) ) ;
#6371 = AXIS2_PLACEMENT_3D ( 'NONE', #6754, #166, #1779 ) ;
#6372 = CARTESIAN_POINT ( 'NONE',  ( -5.787187992231675793, 50.46952898668384790, 78.79017217825926878 ) ) ;
#6373 = FACE_OUTER_BOUND ( 'NONE', #16026, .T. ) ;
#6374 = DIRECTION ( 'NONE',  ( 0.000000000000000000, 0.000000000000000000, 1.000000000000000000 ) ) ;
#6375 = EDGE_CURVE ( 'NONE', #15717, #13055, #2684, .T. ) ;
#6376 = CARTESIAN_POINT ( 'NONE',  ( 9.324313659942287558, 42.73928406446282224, 77.68070116889359156 ) ) ;
#6377 = ORIENTED_EDGE ( 'NONE', *, *, #20787, .F. ) ;
#6378 = CARTESIAN_POINT ( 'NONE',  ( 6.286916181961658801, 38.38547291560929153, 75.79056106475293575 ) ) ;
#6379 = CARTESIAN_POINT ( 'NONE',  ( -3.467962453771612275, 40.50591351489411096, 94.43871379611699979 ) ) ;
#6380 = CARTESIAN_POINT ( 'NONE',  ( 6.539349088566551949, 37.64607664623218142, 78.24541959536460922 ) ) ;
#6381 =( NAMED_UNIT ( * ) PLANE_ANGLE_UNIT ( ) SI_UNIT ( $, .RADIAN. ) );
#6382 = EDGE_CURVE ( 'NONE', #4837, #19613, #1404, .T. ) ;
#6383 = DIRECTION ( 'NONE',  ( 1.334402673828313339E-16, 1.619179559944692391E-32, -1.000000000000000000 ) ) ;
#6384 = VERTEX_POINT ( 'NONE', #6283 ) ;
#6385 = LINE ( 'NONE', #14795, #8765 ) ;
#6386 = VECTOR ( 'NONE', #17053, 1000.000000000000000 ) ;
#6387 = EDGE_CURVE ( 'NONE', #14867, #1091, #4373, .T. ) ;
#6388 = ORIENTED_EDGE ( 'NONE', *, *, #17314, .T. ) ;
#6389 = CARTESIAN_POINT ( 'NONE',  ( -5.784195910403845176, 44.99242805365518194, 94.63308880123798872 ) ) ;
#6390 = CARTESIAN_POINT ( 'NONE',  ( 1.352400422481993658, 50.46853102219002096, 94.32058880123798872 ) ) ;
#6391 = CARTESIAN_POINT ( 'NONE',  ( -7.719292346789278447, 47.24975066309455229, 79.05982662974776076 ) ) ;
#6392 = CARTESIAN_POINT ( 'NONE',  ( 5.394152393224890041, 50.75790946820724514, 75.36022115247205022 ) ) ;
#6393 = CARTESIAN_POINT ( 'NONE',  ( 24.43948732994508077, 43.16218137147969003, 76.90433879953101837 ) ) ;
#6394 = ADVANCED_FACE ( 'NONE', ( #4679 ), #15679, .T. ) ;
#6395 = ORIENTED_EDGE ( 'NONE', *, *, #20354, .F. ) ;
#6396 = CARTESIAN_POINT ( 'NONE',  ( 4.947340820402381212, 51.83388853781453776, 77.72408214165703555 ) ) ;
#6397 = VECTOR ( 'NONE', #17141, 1000.000000000000000 ) ;
#6398 = ORIENTED_EDGE ( 'NONE', *, *, #8821, .F. ) ;
#6399 = CARTESIAN_POINT ( 'NONE',  ( -3.569019236227245706, 51.13477558510469834, 75.44813358671753178 ) ) ;
#6400 = CARTESIAN_POINT ( 'NONE',  ( 5.146040402138061687, 40.41782331071202350, 90.30634062920465510 ) ) ;
#6401 = CARTESIAN_POINT ( 'NONE',  ( -2.416137431568557314, 39.07291177436112406, 94.86746380123797451 ) ) ;
#6402 = ORIENTED_EDGE ( 'NONE', *, *, #19357, .T. ) ;
#6403 = CARTESIAN_POINT ( 'NONE',  ( -5.838384959142698172, 50.43294550856981573, 78.14282209630749776 ) ) ;
#6404 = CARTESIAN_POINT ( 'NONE',  ( -5.747619332630492295, 37.85299557360038136, 79.28390783734228364 ) ) ;
#6405 = CARTESIAN_POINT ( 'NONE',  ( -4.300787881984191152, 37.53891540493670931, 78.93441095796421791 ) ) ;
#6406 = CARTESIAN_POINT ( 'NONE',  ( 5.588830122182042004, 51.36004623135520575, 76.07177712439327877 ) ) ;
#6407 = DIRECTION ( 'NONE',  ( -0.3164954110480847627, -0.9485568250056046757, 0.008402649629174620272 ) ) ;
#6408 = ORIENTED_EDGE ( 'NONE', *, *, #1657, .T. ) ;
#6409 = CARTESIAN_POINT ( 'NONE',  ( -3.998026543861774140, 40.70229664527460045, 92.55433879953100984 ) ) ;
#6410 = LINE ( 'NONE', #20877, #18121 ) ;
#6411 = ORIENTED_EDGE ( 'NONE', *, *, #1305, .F. ) ;
#6412 = CARTESIAN_POINT ( 'NONE',  ( 4.140566530694384184, 51.51580520154297460, 78.43496551412393103 ) ) ;
#6413 = CARTESIAN_POINT ( 'NONE',  ( 10.77494014480653917, 42.96218137147968008, 57.80715055817105252 ) ) ;
#6414 = CARTESIAN_POINT ( 'NONE',  ( -5.809877882140231264, 50.45331562208507847, 76.21531548689122815 ) ) ;
#6415 = CARTESIAN_POINT ( 'NONE',  ( -1.590937568396970203, 39.63064243629642647, 94.51683879611698558 ) ) ;
#6416 = DIRECTION ( 'NONE',  ( -1.000000000000000000, 0.000000000000000000, -0.000000000000000000 ) ) ;
#6417 =( BOUNDED_CURVE ( )  B_SPLINE_CURVE ( 3, ( #2594, #8888, #13980, #17172 ),
 .UNSPECIFIED., .F., .F. ) 
 B_SPLINE_CURVE_WITH_KNOTS ( ( 4, 4 ),
 ( 4.518932018683322838, 4.653621299756558471 ),
 .UNSPECIFIED. ) 
 CURVE ( )  GEOMETRIC_REPRESENTATION_ITEM ( )  RATIONAL_B_SPLINE_CURVE ( ( 1.000000000000000000, 0.9984888044037290022, 0.9984888044037290022, 1.000000000000000000 ) ) 
 REPRESENTATION_ITEM ( '' )  );
#6418 = CARTESIAN_POINT ( 'NONE',  ( 29.63948732994508006, 36.35905713404685002, 74.70433879953100131 ) ) ;
#6419 = CARTESIAN_POINT ( 'NONE',  ( 5.278470088661852522, 37.49201410884709418, 77.76022115247205591 ) ) ;
#6420 = CARTESIAN_POINT ( 'NONE',  ( -3.495065479208319559, 36.18912478048144266, 76.62933879953087057 ) ) ;
#6421 = EDGE_LOOP ( 'NONE', ( #16668, #10947, #14862, #18947 ) ) ;
#6422 = CARTESIAN_POINT ( 'NONE',  ( 2.104109567847143314, 52.20160448666339903, 78.53328619179760040 ) ) ;
#6423 = CARTESIAN_POINT ( 'NONE',  ( -3.410233088748519492, 37.04047751613406092, 77.75315568452884918 ) ) ;
#6424 = CIRCLE ( 'NONE', #3382, 4.000000000000003553 ) ;
#6425 = EDGE_LOOP ( 'NONE', ( #12677, #17665, #12469, #8476, #3046, #6076 ) ) ;
#6426 = CARTESIAN_POINT ( 'NONE',  ( -7.775446761845334898, 41.23134052849093223, 78.58228875689293602 ) ) ;
#6427 = DIRECTION ( 'NONE',  ( 1.000000000000000000, 1.402518428993831676E-16, 1.334402673828313339E-16 ) ) ;
#6428 = CARTESIAN_POINT ( 'NONE',  ( 8.198902672654092783, 41.73077399133128296, 75.36120592425527320 ) ) ;
#6429 = ORIENTED_EDGE ( 'NONE', *, *, #1184, .F. ) ;
#6430 = CIRCLE ( 'NONE', #16971, 0.5999999999999998668 ) ;
#6431 = PLANE ( 'NONE',  #2046 ) ;
#6432 = CARTESIAN_POINT ( 'NONE',  ( -7.240840862912148346, 41.96299060810435577, 79.54527856538405217 ) ) ;
#6433 = ORIENTED_EDGE ( 'NONE', *, *, #10247, .F. ) ;
#6434 = DIRECTION ( 'NONE',  ( 0.7071067811865516806, -0.7071067811865433539, 0.000000000000000000 ) ) ;
#6435 = LINE ( 'NONE', #18725, #5753 ) ;
#6436 = CARTESIAN_POINT ( 'NONE',  ( 3.948530577815480225, 39.69684013992245752, 95.64871379953100927 ) ) ;
#6437 = ORIENTED_EDGE ( 'NONE', *, *, #8479, .T. ) ;
#6438 = CARTESIAN_POINT ( 'NONE',  ( -4.200477280862170204, 37.48494518141774279, 77.15538146413656762 ) ) ;
#6439 = CARTESIAN_POINT ( 'NONE',  ( 8.788263343888127466, 41.13270726085054463, 77.24417474779077963 ) ) ;
#6440 = CARTESIAN_POINT ( 'NONE',  ( 0.2860873169776703140, 38.75537135769874197, 93.65746379953097289 ) ) ;
#6441 = VECTOR ( 'NONE', #8552, 1000.000000000000000 ) ;
#6442 = VECTOR ( 'NONE', #3443, 1000.000000000000000 ) ;
#6443 = VERTEX_POINT ( 'NONE', #7687 ) ;
#6444 = LINE ( 'NONE', #8268, #20601 ) ;
#6445 = CARTESIAN_POINT ( 'NONE',  ( 5.630409355376515990, 37.74693565085873104, 75.37982132168592386 ) ) ;
#6446 = CARTESIAN_POINT ( 'NONE',  ( 1.352400422481993658, 50.46853102219002096, 94.32058880123798872 ) ) ;
#6447 = CARTESIAN_POINT ( 'NONE',  ( -0.3080929418689875576, 37.85583172076933778, 92.44558880123798872 ) ) ;
#6448 = EDGE_CURVE ( 'NONE', #15690, #16873, #4482, .T. ) ;
#6449 = CARTESIAN_POINT ( 'NONE',  ( -5.838369852643723767, 50.43295630312090339, 76.72345405564152543 ) ) ;
#6450 = VECTOR ( 'NONE', #8646, 1000.000000000000000 ) ;
#6451 = CARTESIAN_POINT ( 'NONE',  ( -3.349688636638950889, 52.21127678364309332, 76.69845644658968808 ) ) ;
#6452 = CIRCLE ( 'NONE', #8840, 4.000000000000003553 ) ;
#6453 = CARTESIAN_POINT ( 'NONE',  ( 8.787829143201870252, 41.13140593384865440, 77.14698585835439815 ) ) ;
#6454 = LINE ( 'NONE', #9359, #10878 ) ;
#6455 = DIRECTION ( 'NONE',  ( 1.000000000000000000, 0.000000000000000000, 1.196361017915039239E-16 ) ) ;
#6456 = STYLED_ITEM ( 'NONE', ( #1972 ), #4605 ) ;
#6457 = CARTESIAN_POINT ( 'NONE',  ( -4.208268149563465066, 37.46415075985294862, 76.03844061143841770 ) ) ;
#6458 = DIRECTION ( 'NONE',  ( -1.193617070626243484E-16, -1.000000000000000000, -0.000000000000000000 ) ) ;
#6459 = CARTESIAN_POINT ( 'NONE',  ( 2.029186242314200861, 35.35002428291939225, 76.16022115247204738 ) ) ;
#6460 = DIRECTION ( 'NONE',  ( 1.779391786395883536E-16, 5.922860397471805611E-17, -1.000000000000000000 ) ) ;
#6461 = EDGE_LOOP ( 'NONE', ( #18844, #17614, #8565, #5871, #16755, #4749, #13968, #10013, #19634, #2667, #9760, #10701 ) ) ;
#6462 = ADVANCED_FACE ( 'NONE', ( #17675 ), #14524, .F. ) ;
#6463 = AXIS2_PLACEMENT_3D ( 'NONE', #15073, #486, #4955 ) ;
#6464 = ORIENTED_EDGE ( 'NONE', *, *, #1718, .F. ) ;
#6465 = CARTESIAN_POINT ( 'NONE',  ( 7.690600091884840062, 40.18054381350538051, 76.29938702471172007 ) ) ;
#6466 = PLANE ( 'NONE',  #6023 ) ;
#6467 = CARTESIAN_POINT ( 'NONE',  ( 6.923000991621626632, 50.37454795378102546, 78.43783143115764744 ) ) ;
#6468 = DIRECTION ( 'NONE',  ( 1.000000000000000000, -1.110223024625156417E-16, -1.111814006898795283E-16 ) ) ;
#6470 = EDGE_CURVE ( 'NONE', #225, #5416, #5894, .T. ) ;
#6469 = CARTESIAN_POINT ( 'NONE',  ( 4.673174852049361228, 39.63213674411673537, 94.20433879782399345 ) ) ;
#6471 = B_SPLINE_SURFACE_WITH_KNOTS ( 'NONE', 3, 1, ( 
 ( #11433, #17905 ),
 ( #8230, #18433 ),
 ( #8870, #13849 ),
 ( #15356, #7359 ),
 ( #5767, #13750 ),
 ( #15457, #7254 ),
 ( #2479, #15141 ),
 ( #5654, #10476 ),
 ( #2368, #10694 ),
 ( #13535, #20330 ),
 ( #552, #4169 ),
 ( #10371, #12272 ),
 ( #5442, #16841 ),
 ( #20219, #8974 ),
 ( #17156, #18755 ),
 ( #18323, #18538 ),
 ( #10263, #8758 ),
 ( #15248, #3953 ),
 ( #2260, #12161 ),
 ( #2576, #874 ),
 ( #11846, #17054 ),
 ( #13964, #9077 ),
 ( #772, #18642 ),
 ( #4058, #20119 ),
 ( #663, #20006 ),
 ( #12059, #16737 ),
 ( #7035, #16941 ) ),
 .UNSPECIFIED., .F., .F., .F.,
 ( 4, 1, 1, 1, 1, 1, 1, 1, 1, 1, 1, 1, 1, 1, 1, 1, 1, 1, 1, 1, 1, 1, 1, 1, 4 ),
 ( 2, 2 ),
 ( 0.000000000000000000, 0.05524556061070538121, 0.1069179814647366472, 0.1553727729060086771, 0.2000758033479648479, 0.2417614041178833273, 0.2799066487053696317, 0.3152370222690974444, 0.3476361288249658066, 0.3788200842211088548, 0.4103815830948299714, 0.4425365161269811387, 0.4758329365342930384, 0.5105782220665333604, 0.5468313811506283484, 0.5849849847693828764, 0.6253480228319793222, 0.6671656491570584491, 0.7102157423341657339, 0.7546653220675233475, 0.8003710923354008244, 0.8474641787091774514, 0.8966644363699035614, 0.9474646149202431422, 1.000000000000000000 ),
 ( 0.000000000000000000, 1.000000000000000000 ),
 .UNSPECIFIED. ) ;
#6472 = CARTESIAN_POINT ( 'NONE',  ( -3.416655834652597257, 49.09312775381169303, 93.23111517561484618 ) ) ;
#6473 = AXIS2_PLACEMENT_3D ( 'NONE', #11296, #8720, #8404 ) ;
#6474 = DIRECTION ( 'NONE',  ( -1.540237394707283727E-16, -1.793354297423763257E-16, 1.000000000000000000 ) ) ;
#6475 = CARTESIAN_POINT ( 'NONE',  ( 9.324313659942287558, 42.73928406446282224, 77.68070116889359156 ) ) ;
#6476 = CARTESIAN_POINT ( 'NONE',  ( 0.5221537403064985261, 44.16218137147969003, 96.05433879953096721 ) ) ;
#6477 = CARTESIAN_POINT ( 'NONE',  ( -5.784195910403845176, 44.99242805365518194, 93.38308880123798872 ) ) ;
#6478 = VERTEX_POINT ( 'NONE', #9191 ) ;
#6479 = CARTESIAN_POINT ( 'NONE',  ( -5.850799091716244682, 37.92921030530280291, 79.12851299606570876 ) ) ;
#6480 = CARTESIAN_POINT ( 'NONE',  ( -5.838384959142698172, 50.43294550856981573, 78.14282209630749776 ) ) ;
#6481 = DIRECTION ( 'NONE',  ( 1.000000000000000000, 0.000000000000000000, -0.000000000000000000 ) ) ;
#6482 = CARTESIAN_POINT ( 'NONE',  ( 8.365414986285550469, 41.78545958710412833, 77.39218765127517941 ) ) ;
#6483 = CARTESIAN_POINT ( 'NONE',  ( 9.315603341877332966, 42.71317868864986877, 77.73063109826868811 ) ) ;
#6484 = ORIENTED_EDGE ( 'NONE', *, *, #1467, .F. ) ;
#6485 = CARTESIAN_POINT ( 'NONE',  ( 6.851319717782478946, 37.86899943589613571, 76.12774863075016185 ) ) ;
#6486 = AXIS2_PLACEMENT_3D ( 'NONE', #1392, #1606, #3 ) ;
#6487 = DIRECTION ( 'NONE',  ( 1.540237394707284220E-16, 1.793354297423764243E-16, -1.000000000000000000 ) ) ;
#6488 = FACE_OUTER_BOUND ( 'NONE', #1435, .T. ) ;
#6489 = CARTESIAN_POINT ( 'NONE',  ( -6.709242558049761662, 40.29605830358345031, 78.50801527011910252 ) ) ;
#6490 = CARTESIAN_POINT ( 'NONE',  ( 4.928447940121048809, 46.77256777370082830, 92.45433879953093026 ) ) ;
#6491 = VERTEX_POINT ( 'NONE', #9398 ) ;
#6492 = CARTESIAN_POINT ( 'NONE',  ( -4.383592986664169189, 51.47248658876933547, 78.47566305278908771 ) ) ;
#6493 = VERTEX_POINT ( 'NONE', #15883 ) ;
#6494 = CARTESIAN_POINT ( 'NONE',  ( 5.568489401881125289, 48.03437091500646261, 92.91433880123798872 ) ) ;
#6495 = ADVANCED_FACE ( 'NONE', ( #20751 ), #9719, .T. ) ;
#6496 = CARTESIAN_POINT ( 'NONE',  ( 2.813615989083933844, 36.91585811327295374, 72.45433879953085921 ) ) ;
#6497 = CARTESIAN_POINT ( 'NONE',  ( 5.928963754087450688, 43.92611494815086814, 94.90746379611699979 ) ) ;
#6498 = EDGE_CURVE ( 'NONE', #2056, #6135, #13319, .T. ) ;
#6499 = CARTESIAN_POINT ( 'NONE',  ( -1.077846259693496123, 50.16218137147969713, 77.55433879953099563 ) ) ;
#6500 = VECTOR ( 'NONE', #59, 1000.000000000000227 ) ;
#6501 = DIRECTION ( 'NONE',  ( 0.007885122365285381421, 0.9999689119394085113, 1.805443505845558673E-16 ) ) ;
#6502 = ORIENTED_EDGE ( 'NONE', *, *, #20675, .F. ) ;
#6503 = EDGE_CURVE ( 'NONE', #9206, #10690, #6703, .T. ) ;
#6504 = CARTESIAN_POINT ( 'NONE',  ( -4.522047388140565616, 36.94771494725497973, 76.29203488853940485 ) ) ;
#6505 = COLOUR_RGB ( '', 0.08235294, 0.09019608, 0.10196078) ;
#6506 = EDGE_CURVE ( 'NONE', #20749, #2743, #4998, .T. ) ;
#6507 = EDGE_LOOP ( 'NONE', ( #13339, #10070, #18530, #18532 ) ) ;
#6508 = CARTESIAN_POINT ( 'NONE',  ( -7.719684245581981408, 47.24636383256876115, 78.03730287344849614 ) ) ;
#6509 = CARTESIAN_POINT ( 'NONE',  ( -0.9988176903691428077, 49.83852402762217082, 90.80496380123797451 ) ) ;
#6510 = CARTESIAN_POINT ( 'NONE',  ( 5.568489401881125289, 48.03437091500646261, 94.16433880123797451 ) ) ;
#6511 = ORIENTED_EDGE ( 'NONE', *, *, #13749, .T. ) ;
#6512 = B_SPLINE_CURVE_WITH_KNOTS ( 'NONE', 3,
 ( #4619, #6426, #7834, #4833, #11353, #17511, #17609, #4932, #12823, #11454, #4522, #58, #3039, #11139 ),
 .UNSPECIFIED., .F., .F.,
 ( 4, 2, 2, 2, 2, 2, 4 ),
 ( 0.000000000000000000, 9.720882473674754556E-05, 0.0001944176494734950911, 0.0003888352989470360982, 0.0007776705978941266233, 0.001555341195788341934, 0.003110682391576773641 ),
 .UNSPECIFIED. ) ;
#6513 = CARTESIAN_POINT ( 'NONE',  ( -5.721665869871382704, 50.51634869640449210, 78.97495844722888592 ) ) ;
#6514 = CARTESIAN_POINT ( 'NONE',  ( -5.955451856753747997, 38.00651308716548726, 78.53742703482498655 ) ) ;
#6515 = CARTESIAN_POINT ( 'NONE',  ( 4.393996117251955269, 36.11308595931626542, 76.96022115247204454 ) ) ;
#6516 = DIRECTION ( 'NONE',  ( 1.540237394707284220E-16, 1.793354297423764243E-16, -1.000000000000000000 ) ) ;
#6517 = CARTESIAN_POINT ( 'NONE',  ( 0.5221537403065006355, 44.16218137147969003, 92.45433879953097289 ) ) ;
#6518 = ORIENTED_EDGE ( 'NONE', *, *, #9988, .T. ) ;
#6519 = FACE_OUTER_BOUND ( 'NONE', #8805, .T. ) ;
#6520 = CARTESIAN_POINT ( 'NONE',  ( 0.4414257598867362131, 52.36183294059821947, 76.96012364693363850 ) ) ;
#6521 = AXIS2_PLACEMENT_3D ( 'NONE', #5397, #11919, #13713 ) ;
#6522 = ORIENTED_EDGE ( 'NONE', *, *, #19210, .T. ) ;
#6523 = CARTESIAN_POINT ( 'NONE',  ( 4.172718597472855784, 51.49205576497796244, 78.11943565213420015 ) ) ;
#6524 = CARTESIAN_POINT ( 'NONE',  ( -7.596864591047396864, 40.63365867659160102, 77.28168744664917256 ) ) ;
#6525 = CIRCLE ( 'NONE', #18424, 4.000000000000000000 ) ;
#6526 = CARTESIAN_POINT ( 'NONE',  ( -4.454500421143473332, 37.64505674804929924, 79.54845644658969661 ) ) ;
#6527 = CARTESIAN_POINT ( 'NONE',  ( -4.176309363623031956, 42.45208065485131499, 95.61058879611698558 ) ) ;
#6528 = CARTESIAN_POINT ( 'NONE',  ( 2.921181103050040306, 49.30691215337508737, 90.84496379782399345 ) ) ;
#6529 = CARTESIAN_POINT ( 'NONE',  ( 28.52215374030649642, 44.16218137147969003, 105.5543387995310098 ) ) ;
#6530 = LINE ( 'NONE', #9846, #9936 ) ;
#6531 = CARTESIAN_POINT ( 'NONE',  ( 5.865470552710490892, 51.15570308908012009, 76.01152026380901816 ) ) ;
#6532 = ORIENTED_EDGE ( 'NONE', *, *, #16399, .F. ) ;
#6533 = EDGE_CURVE ( 'NONE', #1116, #14804, #6385, .T. ) ;
#6534 = DIRECTION ( 'NONE',  ( 1.084202172485505420E-16, 1.000000000000000000, 0.000000000000000000 ) ) ;
#6535 = LINE ( 'NONE', #14418, #3194 ) ;
#6536 = VERTEX_POINT ( 'NONE', #16191 ) ;
#6537 = AXIS2_PLACEMENT_3D ( 'NONE', #17181, #5469, #18563 ) ;
#6538 = CARTESIAN_POINT ( 'NONE',  ( 1.630627053521187531, 49.16218137147969003, 92.99615272619178086 ) ) ;
#6539 = VECTOR ( 'NONE', #10340, 1000.000000000000000 ) ;
#6540 = CARTESIAN_POINT ( 'NONE',  ( -1.477846259693495146, 49.81903562097207327, 85.15433879953098995 ) ) ;
#6541 = DIRECTION ( 'NONE',  ( 1.000000000000000000, -0.000000000000000000, 0.000000000000000000 ) ) ;
#6542 = ORIENTED_EDGE ( 'NONE', *, *, #16267, .F. ) ;
#6543 = CARTESIAN_POINT ( 'NONE',  ( 3.460444912181559474, 49.25145096859824889, 94.39871380123798872 ) ) ;
#6544 = CARTESIAN_POINT ( 'NONE',  ( -5.338436749040046614, 37.55074888198199545, 75.45005776384208218 ) ) ;
#6545 = ORIENTED_EDGE ( 'NONE', *, *, #16864, .F. ) ;
#6546 = LINE ( 'NONE', #19526, #19285 ) ;
#6547 = CARTESIAN_POINT ( 'NONE',  ( -4.156531397120291516, 37.43235895057341622, 76.50360254650976799 ) ) ;
#6548 = CARTESIAN_POINT ( 'NONE',  ( -4.500660556396669065, 42.81632233694663370, 92.75808879953098085 ) ) ;
#6549 = EDGE_LOOP ( 'NONE', ( #16969, #9008, #20349, #10413 ) ) ;
#6550 = CARTESIAN_POINT ( 'NONE',  ( -4.270971958021394066, 37.53701675973645280, 77.24798498253255730 ) ) ;
#6551 = CARTESIAN_POINT ( 'NONE',  ( -4.146809383516695036, 37.44530286752341652, 78.34992703482498655 ) ) ;
#6552 = B_SPLINE_CURVE_WITH_KNOTS ( 'NONE', 3,
 ( #888, #7374, #18868, #20460, #5784, #4381, #993, #15372, #10709, #12289, #18769, #7486, #5667, #12177 ),
 .UNSPECIFIED., .F., .F.,
 ( 4, 2, 2, 2, 2, 2, 4 ),
 ( 0.000000000000000000, 0.0002546807491738087856, 0.0005093614983476175712, 0.0007640422475214262484, 0.001018722996695235142, 0.001528084495042833632, 0.002037445993390432555 ),
 .UNSPECIFIED. ) ;
#6553 = VERTEX_POINT ( 'NONE', #1617 ) ;
#6554 = CYLINDRICAL_SURFACE ( 'NONE', #4316, 6.199999999999999289 ) ;
#6555 = CARTESIAN_POINT ( 'NONE',  ( 0.5221537403065071858, 44.16218137147969713, 69.55433879953100984 ) ) ;
#6556 = CARTESIAN_POINT ( 'NONE',  ( 6.198496396448986090, 45.68315280215533392, 94.08621380123798872 ) ) ;
#6557 =( BOUNDED_CURVE ( )  B_SPLINE_CURVE ( 2, ( #6869, #13785, #815, #13375, #10409, #11887, #16778, #20055, #3678, #15175, #10512 ),
 .UNSPECIFIED., .F., .F. ) 
 B_SPLINE_CURVE_WITH_KNOTS ( ( 3, 2, 2, 2, 2, 3 ),
 ( 0.6423390146554854852, 0.6562500000000000000, 0.6875000000000000000, 0.7187500000000000000, 0.7500000000000000000, 0.7673390146554853741 ),
 .UNSPECIFIED. ) 
 CURVE ( )  GEOMETRIC_REPRESENTATION_ITEM ( )  RATIONAL_B_SPLINE_CURVE ( ( 0.9623977609649205789, 0.9661148573551012753, 1.000000000000000000, 0.9238795325112867385, 1.000000000000000000, 0.9238795325112867385, 1.000000000000000000, 0.9238795325112867385, 1.000000000000000000, 0.9577646751561856853, 0.9623977609649205789 ) ) 
 REPRESENTATION_ITEM ( '' )  );
#6558 = AXIS2_PLACEMENT_3D ( 'NONE', #4573, #11095, #14868 ) ;
#6559 = SHAPE_REPRESENTATION_RELATIONSHIP ( 'NONE' , 'NONE' ,  #9739, #13412 ) ;
#6560 = CARTESIAN_POINT ( 'NONE',  ( 1.038073682718705371, 52.33964046710553930, 76.77289608131282250 ) ) ;
#6561 = CARTESIAN_POINT ( 'NONE',  ( 5.665287683258889651, 37.02150436742986273, 75.36022115247205022 ) ) ;
#6562 = DIRECTION ( 'NONE',  ( -1.402518428993831183E-16, 1.000000000000000000, -3.469446951953617640E-16 ) ) ;
#6563 = ORIENTED_EDGE ( 'NONE', *, *, #12873, .F. ) ;
#6564 = CARTESIAN_POINT ( 'NONE',  ( -5.464671512499847061, 38.55876153151410080, 76.02256373304906845 ) ) ;
#6565 = CARTESIAN_POINT ( 'NONE',  ( 8.643446883273359305, 43.06310119191608976, 76.54645538997905874 ) ) ;
#6566 = CARTESIAN_POINT ( 'NONE',  ( 0.5658429483755761380, 52.35438129105421723, 77.38474949312757190 ) ) ;
#6567 = CARTESIAN_POINT ( 'NONE',  ( 6.545534159973747990, 50.65336749702785113, 77.68963291717794561 ) ) ;
#6568 = VERTEX_POINT ( 'NONE', #4892 ) ;
#6569 = VECTOR ( 'NONE', #6369, 1000.000000000000000 ) ;
#6570 = CARTESIAN_POINT ( 'NONE',  ( 5.541932868547512214, 50.64157186687718593, 78.62249727093715990 ) ) ;
#6571 = ORIENTED_EDGE ( 'NONE', *, *, #6591, .T. ) ;
#6572 = EDGE_CURVE ( 'NONE', #6821, #11879, #11478, .T. ) ;
#6573 = DIRECTION ( 'NONE',  ( -1.540237394707284220E-16, -1.793354297423764243E-16, 1.000000000000000000 ) ) ;
#6574 = CARTESIAN_POINT ( 'NONE',  ( 5.427780505986065762, 36.85179043424346190, 77.43080938776617472 ) ) ;
#6575 = DIRECTION ( 'NONE',  ( -1.540237394707284220E-16, -1.793354297423764243E-16, 1.000000000000000000 ) ) ;
#6576 = CARTESIAN_POINT ( 'NONE',  ( -5.547796066657372904, 44.57707013197675394, 94.98020409461749125 ) ) ;
#6577 = DIRECTION ( 'NONE',  ( -0.000000000000000000, 0.000000000000000000, -1.000000000000000000 ) ) ;
#6578 = CARTESIAN_POINT ( 'NONE',  ( 9.304727838458644484, 42.68058411497499804, 77.77798975163413786 ) ) ;
#6579 = CARTESIAN_POINT ( 'NONE',  ( 4.621588727139584130, 51.26391586304784198, 77.68963291717793140 ) ) ;
#6580 = EDGE_CURVE ( 'NONE', #165, #15505, #16411, .T. ) ;
#6581 = VECTOR ( 'NONE', #3036, 1000.000000000000000 ) ;
#6582 = CARTESIAN_POINT ( 'NONE',  ( 6.198496396448986090, 45.68315280215533392, 90.33621380123798872 ) ) ;
#6583 = ORIENTED_EDGE ( 'NONE', *, *, #1526, .F. ) ;
#6584 = CARTESIAN_POINT ( 'NONE',  ( -5.428519676309861985, 37.61728951159455647, 79.46937556254052026 ) ) ;
#6585 = CARTESIAN_POINT ( 'NONE',  ( 8.641007280878683972, 43.01131509312123313, 76.04687335640809920 ) ) ;
#6586 = CARTESIAN_POINT ( 'NONE',  ( 8.345005557250493311, 41.72429123353602165, 77.48121952543638713 ) ) ;
#6587 = CARTESIAN_POINT ( 'NONE',  ( 8.401796425420881675, 39.97444138920005230, 76.12035193564865665 ) ) ;
#6588 = ORIENTED_EDGE ( 'NONE', *, *, #11204, .F. ) ;
#6589 = ORIENTED_EDGE ( 'NONE', *, *, #17493, .T. ) ;
#6590 = CARTESIAN_POINT ( 'NONE',  ( 6.437297979933394032, 38.49293024261085350, 76.32925572521180868 ) ) ;
#6591 = EDGE_CURVE ( 'NONE', #12515, #10923, #16567, .T. ) ;
#6592 = CARTESIAN_POINT ( 'NONE',  ( -1.187946976321872405, 48.86064447540922373, 94.04808879611699979 ) ) ;
#6593 = CARTESIAN_POINT ( 'NONE',  ( 8.139872831506870909, 41.12499011683758710, 79.51301525321822794 ) ) ;
#6594 = CARTESIAN_POINT ( 'NONE',  ( -1.403474231502331637, 49.90122385011594730, 72.45433879953087342 ) ) ;
#6595 = CARTESIAN_POINT ( 'NONE',  ( -0.02883801100815608018, 35.36625256049322275, 79.45433879953087342 ) ) ;
#6596 = EDGE_LOOP ( 'NONE', ( #10347, #5491, #5181, #17782, #6916, #10098, #15475, #12602, #19478, #4398, #10638, #13587, #6213, #5793, #3874, #14899, #9512, #20658, #2529, #17119, #19071, #8494, #19166, #6715, #18883, #14419, #659, #18939, #8255, #18210 ) ) ;
#6597 = CARTESIAN_POINT ( 'NONE',  ( 5.902048492000326441, 51.12868443877599134, 78.59183879953087626 ) ) ;
#6598 = ORIENTED_EDGE ( 'NONE', *, *, #17656, .T. ) ;
#6599 = CARTESIAN_POINT ( 'NONE',  ( 5.544968037009670780, 45.50804040601273925, 94.94558880294498238 ) ) ;
#6600 = CARTESIAN_POINT ( 'NONE',  ( 0.3282210660296583371, 52.35988776924397570, 76.39696619987448400 ) ) ;
#6601 = LINE ( 'NONE', #3421, #8645 ) ;
#6602 = EDGE_CURVE ( 'NONE', #17901, #16856, #10130, .T. ) ;
#6603 = DIRECTION ( 'NONE',  ( 5.626130192357176673E-16, 1.831515347669941892E-30, -1.000000000000000000 ) ) ;
#6604 = EDGE_CURVE ( 'NONE', #20173, #13226, #11517, .T. ) ;
#6605 = CARTESIAN_POINT ( 'NONE',  ( -3.777846259693486974, 36.96218137147968008, 54.55433879953099563 ) ) ;
#6606 = ORIENTED_EDGE ( 'NONE', *, *, #11455, .F. ) ;
#6607 = EDGE_LOOP ( 'NONE', ( #18456, #955, #18242, #16770 ) ) ;
#6608 = DIRECTION ( 'NONE',  ( 1.000000000000000000, 0.000000000000000000, 0.000000000000000000 ) ) ;
#6609 = CARTESIAN_POINT ( 'NONE',  ( -4.567115856812060670, 47.10047254335474065, 92.21121380123797451 ) ) ;
#6610 = CARTESIAN_POINT ( 'NONE',  ( 6.198496396448986090, 45.68315280215533392, 94.08621380123798872 ) ) ;
#6611 = ORIENTED_EDGE ( 'NONE', *, *, #16614, .F. ) ;
#6612 = ADVANCED_FACE ( 'NONE', ( #8644 ), #2460, .T. ) ;
#6613 = CARTESIAN_POINT ( 'NONE',  ( -5.827090762987216621, 50.44101592763561115, 78.49957729094111869 ) ) ;
#6614 = EDGE_CURVE ( 'NONE', #5547, #6239, #8953, .T. ) ;
#6615 = CARTESIAN_POINT ( 'NONE',  ( -5.681413420386576263, 37.80409193316262417, 79.34222993022952153 ) ) ;
#6616 = DIRECTION ( 'NONE',  ( -1.540237394707284467E-16, -1.793354297423764243E-16, 1.000000000000000000 ) ) ;
#6617 = DIRECTION ( 'NONE',  ( -0.000000000000000000, 0.000000000000000000, -1.000000000000000000 ) ) ;
#6618 = ADVANCED_FACE ( 'NONE', ( #8529 ), #5637, .F. ) ;
#6619 = DIRECTION ( 'NONE',  ( -1.540237394707283727E-16, -1.793354297423763257E-16, 1.000000000000000000 ) ) ;
#6620 = VERTEX_POINT ( 'NONE', #18522 ) ;
#6621 = CARTESIAN_POINT ( 'NONE',  ( -4.536263512923754959, 51.36339382032895884, 75.97373057797423712 ) ) ;
#6622 = CARTESIAN_POINT ( 'NONE',  ( 0.8497199531031915942, 52.96350053290503013, 78.59044740879555491 ) ) ;
#6623 = EDGE_LOOP ( 'NONE', ( #13869, #16805, #18249, #473 ) ) ;
#6624 = CARTESIAN_POINT ( 'NONE',  ( 4.577225057937400976, 52.10727814237509392, 78.46169174070733732 ) ) ;
#6625 = CARTESIAN_POINT ( 'NONE',  ( -7.419840600255425578, 40.07385322379796833, 78.42124021397933120 ) ) ;
#6626 = EDGE_CURVE ( 'NONE', #2822, #3440, #15228, .T. ) ;
#6627 = B_SPLINE_CURVE_WITH_KNOTS ( 'NONE', 3,
 ( #4045, #15235, #20320, #969, #7133, #13632, #9065, #20108, #759, #16931, #8962, #2354, #10572, #15345, #7348, #5754, #12262, #4158, #10683, #2566, #7458, #13954, #7987 ),
 .UNSPECIFIED., .F., .F.,
 ( 4, 1, 1, 1, 1, 1, 1, 1, 1, 1, 1, 1, 1, 1, 1, 1, 1, 1, 1, 1, 4 ),
 ( 0.000000000000000000, 0.04338402653469398268, 0.08365674416537959013, 0.1211563976680593846, 0.1555788671761421382, 0.1872558283108043675, 0.2159034631954582228, 0.2418665822845563473, 0.2649561893498845744, 0.3085842690520175235, 0.3528342053628863995, 0.3996013663067077837, 0.4488757727682718413, 0.5007062493018590299, 0.5562201143629579292, 0.6158399466276373024, 0.6805899729784313790, 0.7509145939079137078, 0.8273700343273244773, 0.9100784481637514967, 0.9999999999999998890 ),
 .UNSPECIFIED. ) ;
#6628 = EDGE_CURVE ( 'NONE', #12108, #4469, #751, .T. ) ;
#6629 = CARTESIAN_POINT ( 'NONE',  ( -5.050952507338172914, 50.99561590888721696, 75.40305853716382956 ) ) ;
#6630 = CARTESIAN_POINT ( 'NONE',  ( -4.009385194876761815, 46.27527268018315709, 92.95433879611698558 ) ) ;
#6631 = CARTESIAN_POINT ( 'NONE',  ( -4.622577041588895597, 46.56120873422322859, 91.15746379782397923 ) ) ;
#6632 = CARTESIAN_POINT ( 'NONE',  ( 8.119551934336415755, 43.80226376792169418, 72.45432679953087529 ) ) ;
#6633 = EDGE_CURVE ( 'NONE', #2886, #1872, #16783, .T. ) ;
#6634 = LINE ( 'NONE', #6219, #14251 ) ;
#6635 = DIRECTION ( 'NONE',  ( -0.5773502691896252870, 0.5773502691896259531, -0.5773502691896259531 ) ) ;
#6636 = ORIENTED_EDGE ( 'NONE', *, *, #5161, .F. ) ;
#6637 = PLANE ( 'NONE',  #17640 ) ;
#6638 = DIRECTION ( 'NONE',  ( -0.9480563259966822143, -0.3181025035073955509, -2.030702297275135124E-16 ) ) ;
#6639 = VERTEX_POINT ( 'NONE', #640 ) ;
#6640 = CARTESIAN_POINT ( 'NONE',  ( -5.412716252285423302, 48.91899944357702879, 72.45432679953087529 ) ) ;
#6641 = LINE ( 'NONE', #365, #17726 ) ;
#6642 = CARTESIAN_POINT ( 'NONE',  ( 0.5886017282102210535, 52.96193049659134999, 78.93669174070734584 ) ) ;
#6643 = B_SPLINE_SURFACE_WITH_KNOTS ( 'NONE', 3, 1, ( 
 ( #13109, #11417 ),
 ( #9717, #11522 ),
 ( #13215, #17890 ),
 ( #16197, #19689 ),
 ( #15021, #13736 ),
 ( #7019, #3938 ),
 ( #5424, #7241 ),
 ( #326, #10359 ),
 ( #16829, #14902 ),
 ( #15233, #646 ),
 ( #7128, #15444 ),
 ( #541, #18528 ),
 ( #10466, #11834 ),
 ( #56, #8037 ),
 ( #7832, #16132 ),
 ( #6423, #17508 ),
 ( #6119, #19201 ),
 ( #19411, #14207 ),
 ( #14523, #1551 ) ),
 .UNSPECIFIED., .F., .F., .F.,
 ( 4, 1, 1, 1, 1, 1, 1, 1, 1, 1, 1, 1, 1, 1, 1, 1, 4 ),
 ( 2, 2 ),
 ( 0.000000000000000000, 0.08150191411353231719, 0.1574413810301363015, 0.2279254944343154510, 0.2925593756674912393, 0.3532811523109508078, 0.4087341836578463616, 0.4609809767707315764, 0.5093835833650265377, 0.5574898171909816735, 0.6095021731789963537, 0.6642568233027335012, 0.7231084493840179706, 0.7857192733158503417, 0.8528940375925012640, 0.9238451209387705809, 1.000000000000000000 ),
 ( 0.000000000000000000, 1.000000000000000000 ),
 .UNSPECIFIED. ) ;
#6644 = ORIENTED_EDGE ( 'NONE', *, *, #4826, .F. ) ;
#6645 = CARTESIAN_POINT ( 'NONE',  ( -4.567115856812060670, 47.10047254335474065, 95.96121380123798872 ) ) ;
#6646 = CARTESIAN_POINT ( 'NONE',  ( 0.2541436421823703995, 38.02374091943176637, 94.04808879782397923 ) ) ;
#6647 = CARTESIAN_POINT ( 'NONE',  ( -5.496597427495279575, 38.60358230014927727, 76.35020017089209432 ) ) ;
#6648 = VERTEX_POINT ( 'NONE', #4038 ) ;
#6649 = LINE ( 'NONE', #16555, #1985 ) ;
#6650 = CARTESIAN_POINT ( 'NONE',  ( 5.599231707071657738, 51.35236299959863970, 78.59183879953087626 ) ) ;
#6651 = EDGE_CURVE ( 'NONE', #1583, #3871, #805, .T. ) ;
#6652 = CARTESIAN_POINT ( 'NONE',  ( -6.709242558049761662, 40.29605830358345031, 78.50801527011910252 ) ) ;
#6653 = ORIENTED_EDGE ( 'NONE', *, *, #10462, .F. ) ;
#6654 = CARTESIAN_POINT ( 'NONE',  ( -4.146809383516695924, 37.44530286752341652, 76.81463291717793140 ) ) ;
#6655 = CYLINDRICAL_SURFACE ( 'NONE', #7824, 1.399999999999998579 ) ;
#6656 = CARTESIAN_POINT ( 'NONE',  ( 0.7582201636353284036, 49.56899138526064519, 93.03246379953100131 ) ) ;
#6657 = ORIENTED_EDGE ( 'NONE', *, *, #14800, .T. ) ;
#6658 = CARTESIAN_POINT ( 'NONE',  ( -4.804644443005473775, 51.17161863374556674, 76.44036821129557779 ) ) ;
#6659 = CARTESIAN_POINT ( 'NONE',  ( 2.029186242314200861, 35.35002428291939225, 76.16022115247204738 ) ) ;
#6660 = EDGE_CURVE ( 'NONE', #15210, #18376, #10675, .T. ) ;
#6661 = DIRECTION ( 'NONE',  ( 0.000000000000000000, -3.608224830031758756E-16, 1.000000000000000000 ) ) ;
#6662 = CARTESIAN_POINT ( 'NONE',  ( 6.062166292594780792, 51.01041186941530015, 75.37891144279687694 ) ) ;
#6663 = CARTESIAN_POINT ( 'NONE',  ( 0.7199301301226463945, 52.96500388823179861, 76.81551440955847454 ) ) ;
#6664 = CARTESIAN_POINT ( 'NONE',  ( 4.521197205061672442, 36.20397919953602184, 75.90366482745062626 ) ) ;
#6665 = EDGE_LOOP ( 'NONE', ( #202, #10076, #11963, #4271 ) ) ;
#6666 = CARTESIAN_POINT ( 'NONE',  ( -5.307285386973724428, 38.39462082443735369, 75.68768371633831293 ) ) ;
#6667 = CARTESIAN_POINT ( 'NONE',  ( 8.630330997359013878, 43.02379204977451366, 76.09591779779900378 ) ) ;
#6668 = CARTESIAN_POINT ( 'NONE',  ( 14.52215374030650175, 44.16218137147969003, 105.5543387995309956 ) ) ;
#6669 = DIRECTION ( 'NONE',  ( -0.8043570849667760481, 0.5941461771851693774, -1.733862608106482338E-17 ) ) ;
#6670 =( REPRESENTATION_RELATIONSHIP ('NONE','NONE', #11365, #7678 ) REPRESENTATION_RELATIONSHIP_WITH_TRANSFORMATION ( #17294 )SHAPE_REPRESENTATION_RELATIONSHIP( ) );
#6671 = ORIENTED_EDGE ( 'NONE', *, *, #4303, .F. ) ;
#6672 = AXIS2_PLACEMENT_3D ( 'NONE', #15675, #9394, #1509 ) ;
#6673 = DIRECTION ( 'NONE',  ( 0.000000000000000000, 0.000000000000000000, -1.000000000000000000 ) ) ;
#6674 = ORIENTED_EDGE ( 'NONE', *, *, #19646, .F. ) ;
#6675 = CARTESIAN_POINT ( 'NONE',  ( 6.522436035574397550, 49.75115376156129798, 72.45433879953087342 ) ) ;
#6676 = CARTESIAN_POINT ( 'NONE',  ( 4.566992627068686694, 51.19000347988376376, 77.68963291717794561 ) ) ;
#6677 = DIRECTION ( 'NONE',  ( 0.000000000000000000, 0.000000000000000000, -1.000000000000000000 ) ) ;
#6678 = LINE ( 'NONE', #14668, #1793 ) ;
#6679 = DIRECTION ( 'NONE',  ( -0.7071067811865490160, 1.461539174812751569E-16, 0.7071067811865460184 ) ) ;
#6680 = CARTESIAN_POINT ( 'NONE',  ( 8.865792162213244509, 41.36506604770743678, 78.93669174070734584 ) ) ;
#6681 = LINE ( 'NONE', #8717, #9545 ) ;
#6682 = DIRECTION ( 'NONE',  ( 1.239088197126290817E-16, 1.000000000000000000, 0.000000000000000000 ) ) ;
#6683 = DIRECTION ( 'NONE',  ( -1.000000000000000000, 1.193617070626243484E-16, 0.000000000000000000 ) ) ;
#6684 = VECTOR ( 'NONE', #13859, 1000.000000000000000 ) ;
#6685 = CARTESIAN_POINT ( 'NONE',  ( 3.460444912181559474, 49.25145096859824889, 91.74246380123798872 ) ) ;
#6686 = ORIENTED_EDGE ( 'NONE', *, *, #5989, .T. ) ;
#6687 = CARTESIAN_POINT ( 'NONE',  ( 5.755371611800503828, 51.23702874167446453, 77.28963291717792572 ) ) ;
#6688 = B_SPLINE_CURVE_WITH_KNOTS ( 'NONE', 3,
 ( #20737, #19465, #11403, #1502, #20940, #9384, #15870, #12876, #19358, #17773, #12676, #9702, #19157, #16181, #17872, #3294, #4568, #205, #1913, #18289, #19977, #10116 ),
 .UNSPECIFIED., .F., .F.,
 ( 4, 3, 3, 3, 3, 3, 3, 4 ),
 ( 0.000000000000000000, 0.0001160541354670015593, 0.0002104287037779740748, 0.0002730688264539837622, 0.0003158076471914563312, 0.0003585748116541222349, 0.0004150858277573699594, 0.0004567865026589477636 ),
 .UNSPECIFIED. ) ;
#6689 = ORIENTED_EDGE ( 'NONE', *, *, #10424, .T. ) ;
#6690 = CARTESIAN_POINT ( 'NONE',  ( 8.951667845840693971, 41.62244091939069790, 78.41904468188381827 ) ) ;
#6691 = LINE ( 'NONE', #5097, #14655 ) ;
#6692 = LINE ( 'NONE', #109, #12925 ) ;
#6693 = CARTESIAN_POINT ( 'NONE',  ( 8.385679600361122255, 39.92613824206362949, 77.13595644658970230 ) ) ;
#6694 = ORIENTED_EDGE ( 'NONE', *, *, #16529, .F. ) ;
#6695 = EDGE_LOOP ( 'NONE', ( #16981, #17405, #3944, #18804, #2947, #19278 ) ) ;
#6696 = CARTESIAN_POINT ( 'NONE',  ( 6.490738213730996797, 37.61134109483241872, 75.55565825109377442 ) ) ;
#6697 = CIRCLE ( 'NONE', #2291, 8.199999999999999289 ) ;
#6698 = DIRECTION ( 'NONE',  ( -0.9485903129789527988, 0.3165065846431829311, -8.934458285744989980E-17 ) ) ;
#6699 = CARTESIAN_POINT ( 'NONE',  ( 6.281388312303515242, 38.38152290233981745, 78.07897440853361104 ) ) ;
#6700 = FACE_OUTER_BOUND ( 'NONE', #6507, .T. ) ;
#6701 = DIRECTION ( 'NONE',  ( -1.540237394707283727E-16, -1.793354297423763257E-16, 1.000000000000000000 ) ) ;
#6702 = ORIENTED_EDGE ( 'NONE', *, *, #8600, .F. ) ;
#6703 = LINE ( 'NONE', #17883, #13856 ) ;
#6704 = CARTESIAN_POINT ( 'NONE',  ( -6.427915807670530945, 42.26053564693651055, 78.50654468188380974 ) ) ;
#6705 = VERTEX_POINT ( 'NONE', #5418 ) ;
#6706 = CARTESIAN_POINT ( 'NONE',  ( -2.077846259693550746, 39.65884927180063357, 95.72683880294496817 ) ) ;
#6707 = VECTOR ( 'NONE', #14362, 1000.000000000000000 ) ;
#6708 = CARTESIAN_POINT ( 'NONE',  ( 1.959996514334737094, 52.20282393683998379, 77.13040333250513925 ) ) ;
#6709 = CARTESIAN_POINT ( 'NONE',  ( 5.220616844236030119, 45.87228208810806507, 94.98558879611698558 ) ) ;
#6710 = EDGE_CURVE ( 'NONE', #15999, #4990, #2347, .T. ) ;
#6711 = AXIS2_PLACEMENT_3D ( 'NONE', #13392, #2208, #3901 ) ;
#6712 = DIRECTION ( 'NONE',  ( 0.8136266022444372803, 0.5813877811927012917, 2.295812393977109100E-16 ) ) ;
#6713 = ORIENTED_EDGE ( 'NONE', *, *, #3990, .T. ) ;
#6714 = PLANE ( 'NONE',  #15349 ) ;
#6715 = ORIENTED_EDGE ( 'NONE', *, *, #5321, .F. ) ;
#6716 = CARTESIAN_POINT ( 'NONE',  ( -7.585658068012925526, 47.58366583380566794, 78.31170846932076302 ) ) ;
#6717 = CARTESIAN_POINT ( 'NONE',  ( 2.900946498003601270, 49.13729913812269245, 94.63297921192028639 ) ) ;
#6718 = LINE ( 'NONE', #13225, #17310 ) ;
#6719 = ORIENTED_EDGE ( 'NONE', *, *, #10339, .T. ) ;
#6720 = CARTESIAN_POINT ( 'NONE',  ( -3.154801521863568325, 47.83913663364971569, 92.86286078555453116 ) ) ;
#6721 = CARTESIAN_POINT ( 'NONE',  ( 8.874399228141724549, 41.39086197031718228, 75.36031793586835192 ) ) ;
#6722 = VECTOR ( 'NONE', #1496, 1000.000000000000114 ) ;
#6723 = CARTESIAN_POINT ( 'NONE',  ( 5.865470552710490892, 51.15570308908012009, 76.01152026380901816 ) ) ;
#6724 = EDGE_CURVE ( 'NONE', #10499, #11154, #2662, .T. ) ;
#6725 = CARTESIAN_POINT ( 'NONE',  ( -4.804644443005472887, 51.17161863374555963, 76.44036821129557779 ) ) ;
#6726 = CARTESIAN_POINT ( 'NONE',  ( -3.134114116279072881, 48.15229756555780227, 93.18871379953097289 ) ) ;
#6727 = EDGE_LOOP ( 'NONE', ( #14299, #2919, #17596, #10470 ) ) ;
#6728 = CARTESIAN_POINT ( 'NONE',  ( -4.070368663726195990, 50.94938978984617961, 76.03815620566271605 ) ) ;
#6729 = ORIENTED_EDGE ( 'NONE', *, *, #3008, .F. ) ;
#6730 = CARTESIAN_POINT ( 'NONE',  ( 27.03948732994508930, 36.35905713404685713, 77.50433879953099847 ) ) ;
#6731 = CARTESIAN_POINT ( 'NONE',  ( -6.708915498156351020, 40.30975170697517029, 78.33343394419354411 ) ) ;
#6732 = EDGE_CURVE ( 'NONE', #16948, #3254, #17532, .T. ) ;
#6733 = CARTESIAN_POINT ( 'NONE',  ( 28.52215374030649642, 44.16218137147969003, 87.85433879953103542 ) ) ;
#6734 = CARTESIAN_POINT ( 'NONE',  ( 2.635245049009967921, 48.69372030666295359, 95.14183879611698558 ) ) ;
#6735 = CARTESIAN_POINT ( 'NONE',  ( -1.419351766502867873, 49.49642391118513274, 93.50121379782397923 ) ) ;
#6737 = EDGE_CURVE ( 'NONE', #2084, #5762, #4349, .T. ) ;
#6736 = CARTESIAN_POINT ( 'NONE',  ( -7.032228721109727410, 47.19407273119308144, 78.27541057140679470 ) ) ;
#6738 = ADVANCED_FACE ( 'NONE', ( #20427 ), #15963, .F. ) ;
#6739 = AXIS2_PLACEMENT_3D ( 'NONE', #20004, #13646, #5555 ) ;
#6740 = CARTESIAN_POINT ( 'NONE',  ( -4.307156007511903084, 51.52710565553512367, 75.38014013087713749 ) ) ;
#6741 = ORIENTED_EDGE ( 'NONE', *, *, #11342, .T. ) ;
#6742 = DIRECTION ( 'NONE',  ( 0.8191520442889929088, -0.5735764363510447161, 1.093078678171161153E-16 ) ) ;
#6743 = DIRECTION ( 'NONE',  ( -1.779391786395883536E-16, -5.922860397471805611E-17, 1.000000000000000000 ) ) ;
#6744 = ORIENTED_EDGE ( 'NONE', *, *, #17191, .F. ) ;
#6745 = DIRECTION ( 'NONE',  ( -0.000000000000000000, -0.000000000000000000, 1.000000000000000000 ) ) ;
#6746 = EDGE_CURVE ( 'NONE', #10457, #18032, #18836, .T. ) ;
#6747 = PLANE ( 'NONE',  #17395 ) ;
#6748 = CARTESIAN_POINT ( 'NONE',  ( 1.256812508749381774, 49.74246873332880625, 93.61746379953098085 ) ) ;
#6749 = CARTESIAN_POINT ( 'NONE',  ( -8.220401128834293303, 42.60303496164632264, 76.44005692701139765 ) ) ;
#6750 = ORIENTED_EDGE ( 'NONE', *, *, #5232, .F. ) ;
#6751 =( NAMED_UNIT ( * ) PLANE_ANGLE_UNIT ( ) SI_UNIT ( $, .RADIAN. ) );
#6752 = CARTESIAN_POINT ( 'NONE',  ( -4.834768248550904701, 37.17870924967544255, 75.36094808373545106 ) ) ;
#6753 = VERTEX_POINT ( 'NONE', #9477 ) ;
#6754 = CARTESIAN_POINT ( 'NONE',  ( 31.22215374030650281, 36.96218137147968008, 45.55433879953098852 ) ) ;
#6755 = DIRECTION ( 'NONE',  ( -1.779391786395883536E-16, -5.922860397471806844E-17, 1.000000000000000000 ) ) ;
#6756 = CARTESIAN_POINT ( 'NONE',  ( 5.544968037009670780, 45.50804040601273925, 95.88308879953100927 ) ) ;
#6757 = ORIENTED_EDGE ( 'NONE', *, *, #3797, .T. ) ;
#6758 = CARTESIAN_POINT ( 'NONE',  ( -4.158578283022523081, 37.42937009194851328, 72.45433879953085921 ) ) ;
#6759 = VECTOR ( 'NONE', #12901, 1000.000000000000114 ) ;
#6760 = ORIENTED_EDGE ( 'NONE', *, *, #17215, .F. ) ;
#6761 = CARTESIAN_POINT ( 'NONE',  ( -1.077846259693481024, 49.76218137147968434, 69.55433879953100984 ) ) ;
#6762 = DIRECTION ( 'NONE',  ( 1.110223024625156540E-16, 1.000000000000000000, 5.922860397471808077E-17 ) ) ;
#6763 = EDGE_CURVE ( 'NONE', #17146, #2386, #4245, .T. ) ;
#6764 = CARTESIAN_POINT ( 'NONE',  ( -3.296320189938882983, 36.90521795357528845, 79.15353786348812548 ) ) ;
#6765 = EDGE_CURVE ( 'NONE', #18137, #19468, #10874, .T. ) ;
#6766 = CARTESIAN_POINT ( 'NONE',  ( 4.086113402153771723, 36.81285982569113457, 75.90366482745062626 ) ) ;
#6767 = CIRCLE ( 'NONE', #16307, 6.200000000000000178 ) ;
#6768 = CARTESIAN_POINT ( 'NONE',  ( -1.123656915330052408, 35.37488560990637865, 76.16022115247204738 ) ) ;
#6769 = EDGE_LOOP ( 'NONE', ( #6997, #11559, #670, #5594, #10883, #9873 ) ) ;
#6770 = LINE ( 'NONE', #11896, #18670 ) ;
#6771 = CARTESIAN_POINT ( 'NONE',  ( 8.622345110544836544, 42.99985784037721004, 76.00948821603452643 ) ) ;
#6772 = EDGE_CURVE ( 'NONE', #8020, #11255, #17235, .T. ) ;
#6773 = DIRECTION ( 'NONE',  ( 0.000000000000000000, 0.000000000000000000, 1.000000000000000000 ) ) ;
#6774 = CARTESIAN_POINT ( 'NONE',  ( 9.176231272041631470, 45.98187388689780164, 75.44992703482499508 ) ) ;
#6775 = EDGE_LOOP ( 'NONE', ( #1225, #17691, #3156, #20420 ) ) ;
#6776 = EDGE_CURVE ( 'NONE', #11438, #2175, #7767, .T. ) ;
#6777 = ORIENTED_EDGE ( 'NONE', *, *, #13480, .T. ) ;
#6778 = EDGE_CURVE ( 'NONE', #12733, #7497, #16910, .T. ) ;
#6779 = CIRCLE ( 'NONE', #8825, 8.199999999999995737 ) ;
#6780 = CARTESIAN_POINT ( 'NONE',  ( -1.534364324400819823, 49.45957383111225880, 94.69516862097951559 ) ) ;
#6781 = ORIENTED_EDGE ( 'NONE', *, *, #12361, .T. ) ;
#6782 = CARTESIAN_POINT ( 'NONE',  ( -3.639202304192269644, 36.29559284691161025, 77.48323649892105891 ) ) ;
#6783 = B_SPLINE_CURVE_WITH_KNOTS ( 'NONE', 3,
 ( #1522, #9205, #1111, #19083, #20863, #1210, #19277, #4689, #10910, #7698, #17379, #19175 ),
 .UNSPECIFIED., .F., .F.,
 ( 4, 2, 2, 2, 2, 4 ),
 ( 0.000000000000000000, 0.0001460610222087938687, 0.0002921220444175877374, 0.0003651525555219875584, 0.0004381830666263874879, 0.0005842440888351871841 ),
 .UNSPECIFIED. ) ;
#6784 = CARTESIAN_POINT ( 'NONE',  ( 6.898851416363126710, 50.39238627222024292, 76.00796742194241062 ) ) ;
#6785 = CARTESIAN_POINT ( 'NONE',  ( 9.343936824499609273, 42.79809593351145480, 76.16967972087822147 ) ) ;
#6786 = CARTESIAN_POINT ( 'NONE',  ( 4.809763630234642484, 51.93551126624419112, 77.58315289018165117 ) ) ;
#6787 = CARTESIAN_POINT ( 'NONE',  ( 11.22215374030650281, 51.36218137147968577, 56.80715055817103831 ) ) ;
#6788 = CARTESIAN_POINT ( 'NONE',  ( 5.052198367669452850, 48.31320248322255395, 94.51683879782399345 ) ) ;
#6789 = LINE ( 'NONE', #98, #14187 ) ;
#6790 = VECTOR ( 'NONE', #3867, 1000.000000000000114 ) ;
#6791 = CARTESIAN_POINT ( 'NONE',  ( 4.219159492377686504, 51.44693380490667778, 75.82370277575662953 ) ) ;
#6792 = CARTESIAN_POINT ( 'NONE',  ( -3.350035803220276609, 49.20851703305431357, 90.72683880123797451 ) ) ;
#6793 = VECTOR ( 'NONE', #13687, 1000.000000000000000 ) ;
#6794 = VECTOR ( 'NONE', #9635, 1000.000000000000114 ) ;
#6795 = CARTESIAN_POINT ( 'NONE',  ( -4.524181921268124462, 40.28999182795290324, 92.28933880123798872 ) ) ;
#6796 = AXIS2_PLACEMENT_3D ( 'NONE', #5487, #8695, #18577 ) ;
#6797 = ORIENTED_EDGE ( 'NONE', *, *, #8209, .T. ) ;
#6798 = CARTESIAN_POINT ( 'NONE',  ( 4.732789623540107016, 37.12512171921697046, 75.44058029572614998 ) ) ;
#6799 = CARTESIAN_POINT ( 'NONE',  ( -5.819820656548302829, 50.44621087952127425, 78.57924047249254329 ) ) ;
#6800 = EDGE_CURVE ( 'NONE', #13604, #16684, #2878, .T. ) ;
#6801 = CARTESIAN_POINT ( 'NONE',  ( -4.753421688333181017, 37.11862182248194841, 78.93508260432024315 ) ) ;
#6802 = DIRECTION ( 'NONE',  ( 1.540237394707284220E-16, 1.793354297423764243E-16, -1.000000000000000000 ) ) ;
#6803 = CARTESIAN_POINT ( 'NONE',  ( 30.92220646078100188, 42.96218137147968008, 61.40715055817103263 ) ) ;
#6804 = CARTESIAN_POINT ( 'NONE',  ( 27.67918635042538966, 40.36218137147969287, 87.72755528265716407 ) ) ;
#6805 = ORIENTED_EDGE ( 'NONE', *, *, #17044, .T. ) ;
#6806 = ORIENTED_EDGE ( 'NONE', *, *, #2434, .T. ) ;
#6807 = VECTOR ( 'NONE', #15929, 1000.000000000000000 ) ;
#6808 = DIRECTION ( 'NONE',  ( -0.9585804129707226062, -0.2848220354341972071, -1.987228219138359305E-16 ) ) ;
#6809 = CARTESIAN_POINT ( 'NONE',  ( -6.782631326057146026, 43.38225751353197523, 78.13669174070733447 ) ) ;
#6810 = CARTESIAN_POINT ( 'NONE',  ( 0.7910648968800085834, 52.95821647980518065, 76.03473320275389824 ) ) ;
#6811 = EDGE_LOOP ( 'NONE', ( #5462, #9361, #9978, #7732, #2167, #1569, #17608, #17755, #2986, #15332, #11481, #20563 ) ) ;
#6812 = CARTESIAN_POINT ( 'NONE',  ( 8.951594291416542504, 41.62222047211530906, 76.36070165242202279 ) ) ;
#6813 = CARTESIAN_POINT ( 'NONE',  ( 33.61275266354798674, 36.96218137147968719, 45.55433879953098852 ) ) ;
#6814 = ORIENTED_EDGE ( 'NONE', *, *, #3400, .F. ) ;
#6815 = CARTESIAN_POINT ( 'NONE',  ( -4.500660556396669065, 42.81632233694663370, 95.57058880294496817 ) ) ;
#6816 = CARTESIAN_POINT ( 'NONE',  ( -7.210499118439378741, 41.44819533126688071, 78.81104446281315745 ) ) ;
#6817 = ADVANCED_FACE ( 'NONE', ( #19245 ), #10563, .T. ) ;
#6818 = CARTESIAN_POINT ( 'NONE',  ( -4.567115856812060670, 47.10047254335474065, 94.55496380123798872 ) ) ;
#6819 = B_SPLINE_SURFACE_WITH_KNOTS ( 'NONE', 3, 1, ( 
 ( #12135, #628 ),
 ( #7110, #13613 ),
 ( #8833, #5628 ),
 ( #18613, #4027 ),
 ( #10552, #7759 ),
 ( #2656, #12350 ),
 ( #18722, #11358 ),
 ( #14136, #14039 ),
 ( #12239, #8942 ),
 ( #17338, #17128 ),
 ( #18927, #17228 ) ),
 .UNSPECIFIED., .F., .F., .F.,
 ( 4, 1, 1, 1, 1, 1, 1, 1, 4 ),
 ( 2, 2 ),
 ( 0.000000000000000000, 0.1449716284489762919, 0.2824273770673361716, 0.4139378473324432095, 0.5393048879599185996, 0.6599329406584737434, 0.7760554297062330908, 0.8894112907033583371, 1.000000000000000000 ),
 ( 0.000000000000000000, 1.000000000000000000 ),
 .UNSPECIFIED. ) ;
#6820 = CARTESIAN_POINT ( 'NONE',  ( 8.303614452336031349, 41.57589654819728509, 79.54845644658969661 ) ) ;
#6821 = VERTEX_POINT ( 'NONE', #12865 ) ;
#6822 = CARTESIAN_POINT ( 'NONE',  ( -1.677846259693499542, 47.73989013547934945, 54.55433879953098852 ) ) ;
#6823 = ORIENTED_EDGE ( 'NONE', *, *, #18272, .T. ) ;
#6824 = DIRECTION ( 'NONE',  ( -5.626130192357176673E-16, -1.831515347669941892E-30, 1.000000000000000000 ) ) ;
#6825 = VECTOR ( 'NONE', #16418, 1000.000000000000114 ) ;
#6826 = CARTESIAN_POINT ( 'NONE',  ( -4.567115856812060670, 47.10047254335474065, 95.80496380123798872 ) ) ;
#6827 = VERTEX_POINT ( 'NONE', #6680 ) ;
#6828 = DIRECTION ( 'NONE',  ( 0.5813877811927011807, -0.8136266022444372803, -5.636455622144619183E-17 ) ) ;
#6829 = CARTESIAN_POINT ( 'NONE',  ( -5.368445182934975968, 51.36218137147968577, 80.55433879953099563 ) ) ;
#6830 = CARTESIAN_POINT ( 'NONE',  ( 5.763099067774896334, 42.16033556087237599, 92.55433879953102405 ) ) ;
#6831 = CARTESIAN_POINT ( 'NONE',  ( 2.108290839596759003, 51.34989793853182505, 78.16610350541323271 ) ) ;
#6832 = CARTESIAN_POINT ( 'NONE',  ( -3.467962453771611830, 40.50591351489411096, 93.50121379953097289 ) ) ;
#6833 = ORIENTED_EDGE ( 'NONE', *, *, #4818, .F. ) ;
#6834 = CARTESIAN_POINT ( 'NONE',  ( -4.383574773872678243, 51.47249960296332461, 76.44257241107362688 ) ) ;
#6835 = EDGE_CURVE ( 'NONE', #15434, #17850, #12975, .T. ) ;
#6836 = EDGE_LOOP ( 'NONE', ( #18727, #331, #5075, #12371, #16042 ) ) ;
#6837 = CARTESIAN_POINT ( 'NONE',  ( -4.270168849609139450, 47.18848108112605644, 95.05433879953095300 ) ) ;
#6838 = CARTESIAN_POINT ( 'NONE',  ( -7.949137504989498559, 41.77948864320536160, 78.50654468188380974 ) ) ;
#6839 = CARTESIAN_POINT ( 'NONE',  ( -4.652687709939232086, 51.28020135170361016, 75.36022115247205022 ) ) ;
#6840 = CARTESIAN_POINT ( 'NONE',  ( 2.232254456934871456, 39.46371826755015633, 93.42308879611699979 ) ) ;
#6841 = AXIS2_PLACEMENT_3D ( 'NONE', #18007, #1744, #1630 ) ;
#6842 = CARTESIAN_POINT ( 'NONE',  ( -5.616286711741428128, 44.43019146960381960, 91.39183879782399345 ) ) ;
#6843 = CARTESIAN_POINT ( 'NONE',  ( 5.841953631609400510, 37.14774338596793513, 76.17246542145134924 ) ) ;
#6844 = VECTOR ( 'NONE', #14352, 1000.000000000000000 ) ;
#6845 = EDGE_CURVE ( 'NONE', #7909, #1280, #1282, .T. ) ;
#6846 = ADVANCED_FACE ( 'NONE', ( #7979 ), #5086, .F. ) ;
#6847 = ORIENTED_EDGE ( 'NONE', *, *, #3280, .T. ) ;
#6848 = DIRECTION ( 'NONE',  ( -0.9534635866061470511, -0.3015081906286169455, -2.009271279954808648E-16 ) ) ;
#6849 = PLANE ( 'NONE',  #17380 ) ;
#6850 = ORIENTED_EDGE ( 'NONE', *, *, #16914, .T. ) ;
#6851 = PLANE ( 'NONE',  #19027 ) ;
#6852 = FACE_OUTER_BOUND ( 'NONE', #8541, .T. ) ;
#6853 = CARTESIAN_POINT ( 'NONE',  ( 1.868012774839550749, 39.13936707477651566, 94.32058879953099506 ) ) ;
#6854 = ORIENTED_EDGE ( 'NONE', *, *, #5201, .T. ) ;
#6855 = EDGE_LOOP ( 'NONE', ( #5903, #15697, #6861, #18 ) ) ;
#6856 = VECTOR ( 'NONE', #20263, 1000.000000000000000 ) ;
#6857 = DIRECTION ( 'NONE',  ( -0.5813877811927011807, 0.8136266022444372803, 5.636455622144619183E-17 ) ) ;
#6858 = CARTESIAN_POINT ( 'NONE',  ( 0.5753667321910650445, 52.96202048236657589, 75.97198585835440099 ) ) ;
#6859 = CARTESIAN_POINT ( 'NONE',  ( 6.102441102155617969, 43.42752260303680600, 92.05496379953099506 ) ) ;
#6860 = VECTOR ( 'NONE', #17136, 1000.000000000000000 ) ;
#6861 = ORIENTED_EDGE ( 'NONE', *, *, #14592, .T. ) ;
#6862 =( BOUNDED_CURVE ( )  B_SPLINE_CURVE ( 3, ( #16482, #3495, #13081, #18384 ),
 .UNSPECIFIED., .F., .F. ) 
 B_SPLINE_CURVE_WITH_KNOTS ( ( 4, 4 ),
 ( 5.988669822071448046, 6.577700792287722642 ),
 .UNSPECIFIED. ) 
 CURVE ( )  GEOMETRIC_REPRESENTATION_ITEM ( )  RATIONAL_B_SPLINE_CURVE ( ( 1.000000000000000000, 0.9712952651971044071, 0.9712952651971044071, 1.000000000000000000 ) ) 
 REPRESENTATION_ITEM ( '' )  );
#6863 = LINE ( 'NONE', #4947, #15982 ) ;
#6864 = CARTESIAN_POINT ( 'NONE',  ( 6.198496396448986090, 45.68315280215533392, 94.24246380123798872 ) ) ;
#6865 = ORIENTED_EDGE ( 'NONE', *, *, #15246, .T. ) ;
#6866 = CARTESIAN_POINT ( 'NONE',  ( -4.435470484126775581, 50.68850139621873296, 76.15325518536063498 ) ) ;
#6867 = DIRECTION ( 'NONE',  ( -0.3165065846431826535, -0.9485903129789529098, -2.188653791613874008E-16 ) ) ;
#6868 = CARTESIAN_POINT ( 'NONE',  ( 6.406920570599026199, 49.83092282481639756, 75.87133531663224062 ) ) ;
#6869 = CARTESIAN_POINT ( 'NONE',  ( 0.5221537403065048544, 39.16218137147969003, 93.66636871766883132 ) ) ;
#6870 = VECTOR ( 'NONE', #3769, 1000.000000000000000 ) ;
#6871 = LINE ( 'NONE', #2412, #12662 ) ;
#6872 = EDGE_CURVE ( 'NONE', #2184, #7903, #3083, .T. ) ;
#6873 = ORIENTED_EDGE ( 'NONE', *, *, #13685, .F. ) ;
#6874 = ORIENTED_EDGE ( 'NONE', *, *, #2607, .T. ) ;
#6875 = CARTESIAN_POINT ( 'NONE',  ( 8.318328750355229673, 41.62059619433301094, 75.36022115247205022 ) ) ;
#6876 = VECTOR ( 'NONE', #19763, 1000.000000000000000 ) ;
#6877 = CARTESIAN_POINT ( 'NONE',  ( 8.388854304654358884, 39.93565303222995055, 78.40165754912887053 ) ) ;
#6878 = ORIENTED_EDGE ( 'NONE', *, *, #4563, .T. ) ;
#6879 = DIRECTION ( 'NONE',  ( -1.402518428993831183E-16, 1.000000000000000000, -3.469446951953617640E-16 ) ) ;
#6880 = DIRECTION ( 'NONE',  ( -0.5941461771851693774, -0.8043570849667760481, -2.357623395011396791E-16 ) ) ;
#6881 = CARTESIAN_POINT ( 'NONE',  ( 29.03948732994507864, 45.16218137147969003, 74.70433879953100131 ) ) ;
#6882 = ORIENTED_EDGE ( 'NONE', *, *, #2589, .F. ) ;
#6883 = VERTEX_POINT ( 'NONE', #20929 ) ;
#6884 = CARTESIAN_POINT ( 'NONE',  ( 6.371724945467780898, 50.78175336232117587, 79.44748646226150868 ) ) ;
#6885 = ORIENTED_EDGE ( 'NONE', *, *, #13140, .F. ) ;
#6886 = CARTESIAN_POINT ( 'NONE',  ( 0.4055551487203246652, 52.96467269406713285, 79.54789469633020360 ) ) ;
#6887 = EDGE_CURVE ( 'NONE', #18875, #2898, #3190, .T. ) ;
#6888 = AXIS2_PLACEMENT_3D ( 'NONE', #8546, #13532, #8434 ) ;
#6889 = CARTESIAN_POINT ( 'NONE',  ( 10.77494014480653561, 42.96218137147968008, 69.80574467885101342 ) ) ;
#6891 = ADVANCED_FACE ( 'NONE', ( #1704 ), #16173, .F. ) ;
#6890 = CARTESIAN_POINT ( 'NONE',  ( -7.309558426186682389, 41.73179521895028188, 78.93495393200015542 ) ) ;
#6892 = CARTESIAN_POINT ( 'NONE',  ( -0.7955991294133907266, 52.86330977561153333, 75.91305193028594545 ) ) ;
#6893 = CARTESIAN_POINT ( 'NONE',  ( -4.622577041588896485, 46.56120873422322859, 93.65746379782397923 ) ) ;
#6894 = CARTESIAN_POINT ( 'NONE',  ( 0.8038488827458696306, 52.96385831238255548, 77.48826545068648386 ) ) ;
#6895 = DIRECTION ( 'NONE',  ( 0.000000000000000000, -2.891205793294680792E-16, -1.000000000000000000 ) ) ;
#6896 = CARTESIAN_POINT ( 'NONE',  ( 0.5221537403065086291, 44.16218137147969713, 61.55433879953100273 ) ) ;
#6897 = ADVANCED_FACE ( 'NONE', ( #14464 ), #16383, .T. ) ;
#6898 = CARTESIAN_POINT ( 'NONE',  ( 1.352400422481993658, 50.46853102219002096, 91.82058880123801714 ) ) ;
#6899 = EDGE_CURVE ( 'NONE', #2422, #6639, #15955, .T. ) ;
#6900 = ORIENTED_EDGE ( 'NONE', *, *, #13707, .F. ) ;
#6901 = CARTESIAN_POINT ( 'NONE',  ( 4.481935269463292570, 36.98100317819196192, 75.54009867650407273 ) ) ;
#6902 = AXIS2_PLACEMENT_3D ( 'NONE', #3636, #549, #10149 ) ;
#6903 = ORIENTED_EDGE ( 'NONE', *, *, #2780, .F. ) ;
#6904 = CARTESIAN_POINT ( 'NONE',  ( 1.075234721012297667, 51.35804396568124730, 76.77198585835439815 ) ) ;
#6905 = DIRECTION ( 'NONE',  ( -0.9534635866061452747, -0.3015081906286225522, -2.009271279954815797E-16 ) ) ;
#6906 = CARTESIAN_POINT ( 'NONE',  ( 8.378166699482557433, 41.80998537114106028, 75.36398404145046470 ) ) ;
#6907 = CARTESIAN_POINT ( 'NONE',  ( 6.828503391016846891, 43.33193468930419101, 94.16433880123797451 ) ) ;
#6908 = CARTESIAN_POINT ( 'NONE',  ( 8.371160148690725222, 41.80267820329873274, 77.32525259820312158 ) ) ;
#6909 = DIRECTION ( 'NONE',  ( 4.142850521348543581E-16, -5.922860397471813007E-17, 1.000000000000000000 ) ) ;
#6910 = FACE_OUTER_BOUND ( 'NONE', #16193, .T. ) ;
#6911 = EDGE_LOOP ( 'NONE', ( #312, #19792, #11216, #8422 ) ) ;
#6912 = ORIENTED_EDGE ( 'NONE', *, *, #8373, .F. ) ;
#6913 = CARTESIAN_POINT ( 'NONE',  ( 9.150799720292940975, 42.21925177981464117, 79.41516958226422673 ) ) ;
#6914 = FACE_OUTER_BOUND ( 'NONE', #743, .T. ) ;
#6915 = CARTESIAN_POINT ( 'NONE',  ( -4.158578283022523969, 37.42937009194850617, 78.58080938776616620 ) ) ;
#6916 = ORIENTED_EDGE ( 'NONE', *, *, #5739, .T. ) ;
#6917 = CARTESIAN_POINT ( 'NONE',  ( -4.616483944162940389, 41.91660719363136423, 95.05433879953096721 ) ) ;
#6918 = VECTOR ( 'NONE', #2518, 1000.000000000000227 ) ;
#6919 = CARTESIAN_POINT ( 'NONE',  ( -4.517072128342571880, 36.94403992325788977, 78.58080938776616620 ) ) ;
#6920 = CARTESIAN_POINT ( 'NONE',  ( -0.8237052942265477018, 49.18499566818285018, 94.00808880294498238 ) ) ;
#6921 = ADVANCED_FACE ( 'NONE', ( #16274 ), #8183, .F. ) ;
#6922 = CARTESIAN_POINT ( 'NONE',  ( 2.076668872117770182, 52.20190393242106808, 77.39871602076138402 ) ) ;
#6923 = CARTESIAN_POINT ( 'NONE',  ( -0.9988176903691428077, 49.83852402762217082, 90.80496380123797451 ) ) ;
#6924 = CARTESIAN_POINT ( 'NONE',  ( 8.585425733894268774, 42.66887103129917591, 79.29104084200847069 ) ) ;
#6925 = VERTEX_POINT ( 'NONE', #11497 ) ;
#6926 = CARTESIAN_POINT ( 'NONE',  ( -1.477846259693490261, 50.16218137147969713, 61.15433879953099705 ) ) ;
#6927 = ORIENTED_EDGE ( 'NONE', *, *, #17423, .F. ) ;
#6928 = CARTESIAN_POINT ( 'NONE',  ( -3.226449543290803135, 47.76606447477306716, 95.05433879953076826 ) ) ;
#6929 = CARTESIAN_POINT ( 'NONE',  ( -2.416137431568557314, 39.07291177436112406, 93.61746380123797451 ) ) ;
#6930 = ORIENTED_EDGE ( 'NONE', *, *, #9785, .F. ) ;
#6931 = CARTESIAN_POINT ( 'NONE',  ( 4.512269934384613990, 47.81844922806527620, 92.56371379611699979 ) ) ;
#6932 = CARTESIAN_POINT ( 'NONE',  ( -0.3594811632358371756, 49.16218137147969003, 94.32733169107483207 ) ) ;
#6933 = CARTESIAN_POINT ( 'NONE',  ( 0.5221537403065015237, 44.16218137147968292, 75.45433879953088763 ) ) ;
#6934 = CARTESIAN_POINT ( 'NONE',  ( 0.5221537403065085181, 49.16218137147969003, 93.04136871766880290 ) ) ;
#6935 = ORIENTED_EDGE ( 'NONE', *, *, #7556, .T. ) ;
#6936 = CARTESIAN_POINT ( 'NONE',  ( -1.403474231502331193, 49.90122385011594730, 72.45432679953087529 ) ) ;
#6937 = ORIENTED_EDGE ( 'NONE', *, *, #15127, .F. ) ;
#6938 = PLANE ( 'NONE',  #19587 ) ;
#6939 = CARTESIAN_POINT ( 'NONE',  ( -6.860950806665904622, 40.79053509876318628, 77.37311125041073012 ) ) ;
#6940 = DIRECTION ( 'NONE',  ( -0.3165065846431829311, -0.9485903129789527988, -2.188653791613874255E-16 ) ) ;
#6941 = CARTESIAN_POINT ( 'NONE',  ( 7.863366485876452039, 47.81548183651919004, 78.86171667562430798 ) ) ;
#6942 = CARTESIAN_POINT ( 'NONE',  ( 2.463659247115867146, 38.82793883177424732, 93.03246379782397923 ) ) ;
#6943 = CARTESIAN_POINT ( 'NONE',  ( 5.495247707634323575, 37.64691545862963551, 76.55482881315118959 ) ) ;
#6944 = VERTEX_POINT ( 'NONE', #17969 ) ;
#6945 = DIRECTION ( 'NONE',  ( 0.009567942452870513079, -0.9999542261909885044, -1.778535306010344808E-16 ) ) ;
#6946 = EDGE_CURVE ( 'NONE', #15405, #1280, #6789, .T. ) ;
#6947 = ORIENTED_EDGE ( 'NONE', *, *, #17676, .T. ) ;
#6948 = DIRECTION ( 'NONE',  ( -1.402518428993830937E-16, 1.000000000000000000, -3.469446951953617147E-16 ) ) ;
#6949 = CARTESIAN_POINT ( 'NONE',  ( -2.904223097202481174, 48.62752260303690122, 93.77371379953099506 ) ) ;
#6950 = CARTESIAN_POINT ( 'NONE',  ( -3.943187491250720544, 40.73580453397070755, 92.83621379953099506 ) ) ;
#6951 = ORIENTED_EDGE ( 'NONE', *, *, #6328, .T. ) ;
#6952 = CARTESIAN_POINT ( 'NONE',  ( 31.07218010054375412, 45.56218137147968861, 64.80574467885102763 ) ) ;
#6953 = CARTESIAN_POINT ( 'NONE',  ( -5.507653477476715409, 38.61174895890570724, 76.59693911441793546 ) ) ;
#6954 = VERTEX_POINT ( 'NONE', #19766 ) ;
#6955 = CARTESIAN_POINT ( 'NONE',  ( -4.043113822512209410, 40.96171489760612161, 95.05433879953098142 ) ) ;
#6956 = CARTESIAN_POINT ( 'NONE',  ( 0.3339603559181820169, 52.96017240013473071, 76.18796968951495785 ) ) ;
#6957 = CARTESIAN_POINT ( 'NONE',  ( -5.058133621542618030, 44.89684013992257405, 91.42996379953099506 ) ) ;
#6958 = ORIENTED_EDGE ( 'NONE', *, *, #10062, .F. ) ;
#6959 = CARTESIAN_POINT ( 'NONE',  ( -3.677846259693482445, 44.16218137147969003, 56.15433879953099705 ) ) ;
#6960 = CARTESIAN_POINT ( 'NONE',  ( -5.154188915835984375, 42.64120994080404614, 94.86746380123797451 ) ) ;
#6961 = EDGE_LOOP ( 'NONE', ( #9416, #4110, #9942, #6927 ) ) ;
#6962 = CARTESIAN_POINT ( 'NONE',  ( 0.5868117437017631444, 52.36192644938283536, 77.38375056423674891 ) ) ;
#6963 = LINE ( 'NONE', #13062, #3729 ) ;
#6964 = DIRECTION ( 'NONE',  ( -0.02415648568939433166, -0.9997081895228917547, -3.608224830031758756E-16 ) ) ;
#6965 = CARTESIAN_POINT ( 'NONE',  ( 0.5221537403065117378, 47.36218137147970708, 45.55433879953100273 ) ) ;
#6966 = DIRECTION ( 'NONE',  ( 0.007885122365275663500, 0.9999689119394085113, 1.805443505845543142E-16 ) ) ;
#6967 = ORIENTED_EDGE ( 'NONE', *, *, #11967, .T. ) ;
#6968 = ORIENTED_EDGE ( 'NONE', *, *, #1588, .F. ) ;
#6969 = ADVANCED_FACE ( 'NONE', ( #14991 ), #4075, .F. ) ;
#6970 = FACE_OUTER_BOUND ( 'NONE', #9746, .T. ) ;
#6971 = ADVANCED_FACE ( 'NONE', ( #10217 ), #6126, .T. ) ;
#6972 = ORIENTED_EDGE ( 'NONE', *, *, #6580, .F. ) ;
#6973 = CARTESIAN_POINT ( 'NONE',  ( 0.5221537403065019678, 44.16218137147968292, 72.45433879953087342 ) ) ;
#6974 = FACE_OUTER_BOUND ( 'NONE', #10315, .T. ) ;
#6975 = CARTESIAN_POINT ( 'NONE',  ( -4.524181921268124462, 40.28999182795290324, 94.94558880123797451 ) ) ;
#6976 =( BOUNDED_CURVE ( )  B_SPLINE_CURVE ( 2, ( #5906, #9627, #9214, #14090, #15805, #17588, #6099, #1118, #9415, #7707, #18981 ),
 .UNSPECIFIED., .F., .F. ) 
 B_SPLINE_CURVE_WITH_KNOTS ( ( 3, 2, 2, 2, 2, 3 ),
 ( 0.3923390146554854296, 0.4062500000000000000, 0.4375000000000000000, 0.4687500000000000000, 0.5000000000000000000, 0.5173390146554853741 ),
 .UNSPECIFIED. ) 
 CURVE ( )  GEOMETRIC_REPRESENTATION_ITEM ( )  RATIONAL_B_SPLINE_CURVE ( ( 0.9623977609649205789, 0.9661148573551011642, 1.000000000000000000, 0.9238795325112867385, 1.000000000000000000, 0.9238795325112867385, 1.000000000000000000, 0.9238795325112867385, 1.000000000000000000, 0.9577646751561856853, 0.9623977609649205789 ) ) 
 REPRESENTATION_ITEM ( '' )  );
#6977 = VERTEX_POINT ( 'NONE', #5392 ) ;
#6978 = CARTESIAN_POINT ( 'NONE',  ( -5.368445182934982185, 36.96218137147968008, 53.35433879953099989 ) ) ;
#6979 = ORIENTED_EDGE ( 'NONE', *, *, #5178, .F. ) ;
#6980 = FACE_OUTER_BOUND ( 'NONE', #12517, .T. ) ;
#6981 = EDGE_CURVE ( 'NONE', #15226, #19138, #15199, .T. ) ;
#6982 = CARTESIAN_POINT ( 'NONE',  ( -3.890009847151996603, 51.07470118294932604, 79.52219083255405963 ) ) ;
#6983 = CARTESIAN_POINT ( 'NONE',  ( 8.300594306733913186, 41.56682737740558764, 77.52492703482499792 ) ) ;
#6984 = CARTESIAN_POINT ( 'NONE',  ( -3.350035803220276609, 49.20851703305431357, 95.88308880123798872 ) ) ;
#6985 = B_SPLINE_SURFACE_WITH_KNOTS ( 'NONE', 3, 1, ( 
 ( #4720, #17512 ),
 ( #2934, #1140 ),
 ( #20798, #10938 ),
 ( #20686, #9549 ),
 ( #18901, #16031 ),
 ( #4313, #12824 ),
 ( #9339, #2731 ),
 ( #7835, #1236 ),
 ( #14318, #9234 ),
 ( #14210, #6124 ),
 ( #12627, #19003 ) ),
 .UNSPECIFIED., .F., .F., .F.,
 ( 4, 1, 1, 1, 1, 1, 1, 1, 4 ),
 ( 2, 2 ),
 ( 0.000000000000000000, 0.1895954080786773355, 0.3480750146108056442, 0.4761617831461403827, 0.5797469728315796100, 0.6725800605763750939, 0.7701180849273350226, 0.8764776678571430946, 1.000000000000000000 ),
 ( 0.000000000000000000, 1.000000000000000000 ),
 .UNSPECIFIED. ) ;
#6986 = CARTESIAN_POINT ( 'NONE',  ( 8.285567280566995763, 41.54615094762161931, 75.97281361087948426 ) ) ;
#6987 = DIRECTION ( 'NONE',  ( 4.150711087041459392E-32, -3.469446951953617147E-16, -1.000000000000000000 ) ) ;
#6988 = CARTESIAN_POINT ( 'NONE',  ( 4.661142417382979630, 52.04529176935007939, 75.82370277575662953 ) ) ;
#6989 = CARTESIAN_POINT ( 'NONE',  ( 5.611423337425062385, 41.22389019960463230, 92.67996380123798872 ) ) ;
#6990 = CARTESIAN_POINT ( 'NONE',  ( -7.956575413799908070, 41.77588473132961155, 78.56636689789523587 ) ) ;
#6991 = VERTEX_POINT ( 'NONE', #8026 ) ;
#6992 = EDGE_CURVE ( 'NONE', #16499, #8766, #2641, .T. ) ;
#6993 = CARTESIAN_POINT ( 'NONE',  ( 4.401732967732903568, 36.93750505876209189, 75.58501954835062975 ) ) ;
#6994 = ADVANCED_FACE ( 'NONE', ( #10857 ), #9142, .F. ) ;
#6995 = EDGE_CURVE ( 'NONE', #18032, #7102, #10482, .T. ) ;
#6996 = AXIS2_PLACEMENT_3D ( 'NONE', #15094, #15195, #3803 ) ;
#6997 = ORIENTED_EDGE ( 'NONE', *, *, #6732, .F. ) ;
#6998 = CARTESIAN_POINT ( 'NONE',  ( 5.204008869086888645, 50.89421323063470481, 76.99291999501369332 ) ) ;
#6999 = CARTESIAN_POINT ( 'NONE',  ( 1.215246153217546254, 50.28109722957945849, 67.67325465763076409 ) ) ;
#7000 = CARTESIAN_POINT ( 'NONE',  ( -4.435668263947954770, 37.63854610978014392, 78.92026643871187730 ) ) ;
#7001 = CARTESIAN_POINT ( 'NONE',  ( -4.524181921268124462, 40.28999182795290324, 92.44558880123798872 ) ) ;
#7002 = CARTESIAN_POINT ( 'NONE',  ( -5.160557796315992540, 37.41935686500602287, 77.33669174070733732 ) ) ;
#7003 = CARTESIAN_POINT ( 'NONE',  ( 31.07218010054375412, 42.76218137147968434, 70.80574467885102763 ) ) ;
#7004 = EDGE_CURVE ( 'NONE', #9419, #6493, #18706, .T. ) ;
#7005 = LINE ( 'NONE', #8637, #19339 ) ;
#7006 = B_SPLINE_CURVE_WITH_KNOTS ( 'NONE', 3,
 ( #16059, #17751, #8281, #19546, #19751, #3073 ),
 .UNSPECIFIED., .F., .F.,
 ( 4, 2, 4 ),
 ( 0.000000000000000000, 0.001381092432504991453, 0.002762184865009982906 ),
 .UNSPECIFIED. ) ;
#7007 = ORIENTED_EDGE ( 'NONE', *, *, #11446, .F. ) ;
#7008 = ORIENTED_EDGE ( 'NONE', *, *, #15634, .T. ) ;
#7009 = CARTESIAN_POINT ( 'NONE',  ( 0.5221537403065010796, 44.16218137147968292, 78.18375056423674607 ) ) ;
#7010 = DIRECTION ( 'NONE',  ( -9.598494438985368964E-18, 5.922860397471809309E-17, -1.000000000000000000 ) ) ;
#7011 = DIRECTION ( 'NONE',  ( -1.540237394707284467E-16, -1.793354297423764243E-16, 1.000000000000000000 ) ) ;
#7012 = ORIENTED_EDGE ( 'NONE', *, *, #9722, .F. ) ;
#7013 = CARTESIAN_POINT ( 'NONE',  ( 0.3279640439667346752, 52.35988168082470651, 77.10139762306027933 ) ) ;
#7014 = CARTESIAN_POINT ( 'NONE',  ( -4.250200499057710246, 41.08694408590478986, 95.05433879953098142 ) ) ;
#7015 = VECTOR ( 'NONE', #8640, 1000.000000000000000 ) ;
#7016 = CARTESIAN_POINT ( 'NONE',  ( 28.43948732994508077, 43.16218137147969003, 76.90433879953101837 ) ) ;
#7017 = CARTESIAN_POINT ( 'NONE',  ( -3.981178359372548492, 46.76218137147973408, 90.41433880294496817 ) ) ;
#7018 = CARTESIAN_POINT ( 'NONE',  ( 1.561445875196035615, 52.20596665509935974, 76.85511030890285156 ) ) ;
#7019 = CARTESIAN_POINT ( 'NONE',  ( -3.118155632002933331, 36.82473166443372037, 78.17158301229430606 ) ) ;
#7020 = CARTESIAN_POINT ( 'NONE',  ( -5.784195910403845176, 44.99242805365518194, 91.03933880123798872 ) ) ;
#7021 = UNCERTAINTY_MEASURE_WITH_UNIT (LENGTH_MEASURE( 1.000000000000000082E-05 ), #16252, 'distance_accuracy_value', 'NONE');
#7022 = CARTESIAN_POINT ( 'NONE',  ( -8.188298522726004336, 42.90970694978335587, 78.73977153168188181 ) ) ;
#7023 = ORIENTED_EDGE ( 'NONE', *, *, #17554, .F. ) ;
#7024 = ADVANCED_FACE ( 'NONE', ( #19401 ), #17811, .F. ) ;
#7025 = LINE ( 'NONE', #3630, #6365 ) ;
#7026 = ORIENTED_EDGE ( 'NONE', *, *, #11448, .T. ) ;
#7027 = COLOUR_RGB ( '', 0.72549020, 0.75294118, 0.79215686) ;
#7028 = FACE_OUTER_BOUND ( 'NONE', #19945, .T. ) ;
#7029 = EDGE_CURVE ( 'NONE', #15850, #13342, #4443, .T. ) ;
#7030 = CARTESIAN_POINT ( 'NONE',  ( 5.611423337425062385, 41.22389019960463230, 91.42996380123798872 ) ) ;
#7031 = ORIENTED_EDGE ( 'NONE', *, *, #8307, .F. ) ;
#7032 = LINE ( 'NONE', #19906, #18794 ) ;
#7033 = ADVANCED_FACE ( 'NONE', ( #12221 ), #4118, .F. ) ;
#7034 = DIRECTION ( 'NONE',  ( 1.540237394707284220E-16, 1.793354297423764243E-16, -1.000000000000000000 ) ) ;
#7035 = CARTESIAN_POINT ( 'NONE',  ( -4.574316323987747346, 51.33620267474496757, 79.54845644658969661 ) ) ;
#7036 = CARTESIAN_POINT ( 'NONE',  ( 0.6775615626972071315, 52.96083427075867434, 77.39742084373497732 ) ) ;
#7037 = CARTESIAN_POINT ( 'NONE',  ( 5.605180980092264953, 51.34796851126965578, 77.21343514867072599 ) ) ;
#7038 = DIRECTION ( 'NONE',  ( -0.000000000000000000, -0.000000000000000000, 1.000000000000000000 ) ) ;
#7039 = ORIENTED_EDGE ( 'NONE', *, *, #15179, .F. ) ;
#7040 = LINE ( 'NONE', #1202, #16646 ) ;
#7041 = VECTOR ( 'NONE', #1645, 1000.000000000000000 ) ;
#7042 = ORIENTED_EDGE ( 'NONE', *, *, #18825, .F. ) ;
#7043 = FACE_OUTER_BOUND ( 'NONE', #9193, .T. ) ;
#7044 = CARTESIAN_POINT ( 'NONE',  ( -7.871639067970514603, 41.50258186480986922, 76.21059579996631328 ) ) ;
#7045 = CARTESIAN_POINT ( 'NONE',  ( 6.371724945467780898, 50.78175336232117587, 79.44748646226150868 ) ) ;
#7046 = AXIS2_PLACEMENT_3D ( 'NONE', #7582, #1095, #14265 ) ;
#7047 = CARTESIAN_POINT ( 'NONE',  ( 0.7901638384306293172, 50.30062182352762079, 91.07933879782399345 ) ) ;
#7048 = CARTESIAN_POINT ( 'NONE',  ( 5.494513770740271141, 37.64639101419628986, 76.49330797698027595 ) ) ;
#7049 = ORIENTED_EDGE ( 'NONE', *, *, #848, .F. ) ;
#7050 = CARTESIAN_POINT ( 'NONE',  ( 8.289263307265827052, 41.55743062947783528, 78.93669174070734584 ) ) ;
#7051 = AXIS2_PLACEMENT_3D ( 'NONE', #19054, #15966, #9480 ) ;
#7052 = ORIENTED_EDGE ( 'NONE', *, *, #16128, .T. ) ;
#7053 = FACE_BOUND ( 'NONE', #7761, .T. ) ;
#7054 = CARTESIAN_POINT ( 'NONE',  ( 3.948530577815480225, 39.69684013992245752, 94.39871379953098085 ) ) ;
#7055 = CARTESIAN_POINT ( 'NONE',  ( -4.500660556396669065, 42.81632233694663370, 94.00808879953098085 ) ) ;
#7056 = ORIENTED_EDGE ( 'NONE', *, *, #12747, .T. ) ;
#7057 = LINE ( 'NONE', #8782, #11918 ) ;
#7058 = DIRECTION ( 'NONE',  ( 5.626130192357176673E-16, 1.831515347669941892E-30, -1.000000000000000000 ) ) ;
#7059 = ORIENTED_EDGE ( 'NONE', *, *, #15366, .T. ) ;
#7060 = CARTESIAN_POINT ( 'NONE',  ( -4.463792963332829267, 40.72925446781975722, 72.45433879953085921 ) ) ;
#7061 = CARTESIAN_POINT ( 'NONE',  ( -4.598246518171406727, 51.31910303412164609, 78.93669174070734584 ) ) ;
#7062 = ORIENTED_EDGE ( 'NONE', *, *, #16213, .T. ) ;
#7063 = DIRECTION ( 'NONE',  ( 0.5941461771851692664, 0.8043570849667761591, 2.357623395011396791E-16 ) ) ;
#7064 = CARTESIAN_POINT ( 'NONE',  ( -3.350035803220276609, 49.20851703305431357, 95.88308880123798872 ) ) ;
#7065 = ORIENTED_EDGE ( 'NONE', *, *, #14174, .F. ) ;
#7066 = DIRECTION ( 'NONE',  ( 0.000000000000000000, 1.000000000000000000, 0.000000000000000000 ) ) ;
#7067 = LINE ( 'NONE', #12309, #14945 ) ;
#7068 = CARTESIAN_POINT ( 'NONE',  ( 1.352400422481993658, 50.46853102219002096, 91.82058880123801714 ) ) ;
#7069 = VECTOR ( 'NONE', #20233, 1000.000000000000000 ) ;
#7070 = CARTESIAN_POINT ( 'NONE',  ( 0.000000000000000000, 0.000000000000000000, 0.000000000000000000 ) ) ;
#7071 = CARTESIAN_POINT ( 'NONE',  ( -3.625666805699581108, 36.28559471941820647, 77.96849812480175501 ) ) ;
#7072 = DIRECTION ( 'NONE',  ( -9.598494438985368964E-18, 5.922860397471809309E-17, -1.000000000000000000 ) ) ;
#7073 = LINE ( 'NONE', #490, #10289 ) ;
#7074 = EDGE_CURVE ( 'NONE', #15383, #19989, #1541, .T. ) ;
#7075 = EDGE_LOOP ( 'NONE', ( #5563, #19257, #19837, #1962 ) ) ;
#7076 = EDGE_LOOP ( 'NONE', ( #13473, #15820, #2932, #20763 ) ) ;
#7077 = DIRECTION ( 'NONE',  ( -1.540237394707284467E-16, -1.793354297423764243E-16, 1.000000000000000000 ) ) ;
#7078 = ORIENTED_EDGE ( 'NONE', *, *, #17456, .F. ) ;
#7079 = CARTESIAN_POINT ( 'NONE',  ( -4.682451852912701717, 37.82245906599816010, 75.37232954241834193 ) ) ;
#7080 = PLANE ( 'NONE',  #19449 ) ;
#7081 = DIRECTION ( 'NONE',  ( 0.000000000000000000, 0.000000000000000000, 1.000000000000000000 ) ) ;
#7082 = VERTEX_POINT ( 'NONE', #20607 ) ;
#7083 = CIRCLE ( 'NONE', #12211, 6.200000000000000178 ) ;
#7084 = CARTESIAN_POINT ( 'NONE',  ( 2.522153740306510628, 49.81903562097208038, 53.15433879953100416 ) ) ;
#7085 = ORIENTED_EDGE ( 'NONE', *, *, #20523, .T. ) ;
#7086 = CARTESIAN_POINT ( 'NONE',  ( -7.677846259693481556, 40.96218137147969429, 93.55433879953098142 ) ) ;
#7087 = CARTESIAN_POINT ( 'NONE',  ( 6.447293898846322868, 38.50007296029209414, 76.59354538285809610 ) ) ;
#7088 = B_SPLINE_CURVE_WITH_KNOTS ( 'NONE', 3,
 ( #521, #2231, #12134, #18612, #20301, #5526, #12238, #15430, #12036, #13932, #2551, #18291, #10232, #18510, #845 ),
 .UNSPECIFIED., .F., .F.,
 ( 4, 1, 1, 1, 1, 1, 1, 1, 1, 1, 1, 1, 4 ),
 ( 0.000000000000000000, 0.1167597168375007488, 0.2214683318549902913, 0.3169846747733736647, 0.4005759510517727939, 0.4723184013547362947, 0.5354911787873812834, 0.5872921887835030885, 0.6299408870648134373, 0.7051993628396346914, 0.7869278594151544182, 0.8829706743529757151, 1.000000000000000000 ),
 .UNSPECIFIED. ) ;
#7089 = CARTESIAN_POINT ( 'NONE',  ( -0.4699484075730042676, 52.36218137147968577, 52.53721119516358584 ) ) ;
#7090 = CARTESIAN_POINT ( 'NONE',  ( 4.163798982342816757, 51.48782638361205954, 77.30394856433355244 ) ) ;
#7091 = FACE_OUTER_BOUND ( 'NONE', #545, .T. ) ;
#7092 = CARTESIAN_POINT ( 'NONE',  ( -5.004817973257477348, 39.29348442311233214, 76.73301527011911105 ) ) ;
#7093 = CARTESIAN_POINT ( 'NONE',  ( 0.8396437586116388685, 52.96357605663151702, 77.59858114993788547 ) ) ;
#7094 = CYLINDRICAL_SURFACE ( 'NONE', #2721, 6.000000000000001776 ) ;
#7095 = DIRECTION ( 'NONE',  ( -5.626130192357176673E-16, -1.831515347669941892E-30, 1.000000000000000000 ) ) ;
#7096 = CARTESIAN_POINT ( 'NONE',  ( -0.3080929418689875576, 37.85583172076933778, 91.19558880123798872 ) ) ;
#7097 = AXIS2_PLACEMENT_3D ( 'NONE', #17273, #7904, #4799 ) ;
#7098 = CARTESIAN_POINT ( 'NONE',  ( 8.378029088801538293, 41.81159710496287119, 76.29056865213834726 ) ) ;
#7099 = CARTESIAN_POINT ( 'NONE',  ( 0.3839191465529612213, 52.96715465491344332, 76.04467822456393833 ) ) ;
#7100 =( BOUNDED_CURVE ( )  B_SPLINE_CURVE ( 3, ( #12842, #9982, #11155, #17624 ),
 .UNSPECIFIED., .F., .F. ) 
 B_SPLINE_CURVE_WITH_KNOTS ( ( 4, 4 ),
 ( 4.703063163714124251, 4.858985947692485041 ),
 .UNSPECIFIED. ) 
 CURVE ( )  GEOMETRIC_REPRESENTATION_ITEM ( )  RATIONAL_B_SPLINE_CURVE ( ( 1.000000000000000000, 0.9979750330736136821, 0.9979750330736136821, 1.000000000000000000 ) ) 
 REPRESENTATION_ITEM ( '' )  );
#7101 = CIRCLE ( 'NONE', #19017, 1.399999999999995026 ) ;
#7102 = VERTEX_POINT ( 'NONE', #20508 ) ;
#7103 = CARTESIAN_POINT ( 'NONE',  ( -4.383473025373058718, 51.47257230871590394, 76.47051527011910821 ) ) ;
#7104 = EDGE_CURVE ( 'NONE', #10809, #14970, #18915, .T. ) ;
#7105 = CARTESIAN_POINT ( 'NONE',  ( 0.5221537403065020788, 52.36218137147968577, 83.03825919817350609 ) ) ;
#7106 = CARTESIAN_POINT ( 'NONE',  ( -3.425442721482995445, 52.15714568814760810, 78.86270620133520026 ) ) ;
#7107 = CARTESIAN_POINT ( 'NONE',  ( 1.352400422481993658, 50.46853102219002096, 94.47683880123798872 ) ) ;
#7108 = VECTOR ( 'NONE', #8786, 1000.000000000000000 ) ;
#7109 = CARTESIAN_POINT ( 'NONE',  ( -4.545392591669648930, 36.96495910869975887, 77.09144163344554102 ) ) ;
#7110 = CARTESIAN_POINT ( 'NONE',  ( -6.812698123362908476, 47.79501813703141266, 78.79824701870994375 ) ) ;
#7111 = DIRECTION ( 'NONE',  ( -1.334402673828310381E-16, -2.168404344970984808E-15, 1.000000000000000000 ) ) ;
#7112 = DIRECTION ( 'NONE',  ( -0.3165065846431829311, -0.9485903129789527988, -2.188653791613874255E-16 ) ) ;
#7113 = CIRCLE ( 'NONE', #18685, 1.399999999999995026 ) ;
#7114 = ORIENTED_EDGE ( 'NONE', *, *, #18489, .F. ) ;
#7115 = ORIENTED_EDGE ( 'NONE', *, *, #13140, .T. ) ;
#7116 = VECTOR ( 'NONE', #3761, 1000.000000000000000 ) ;
#7117 = CARTESIAN_POINT ( 'NONE',  ( 8.316824854331539285, 42.08419425066229991, 79.51559944055343010 ) ) ;
#7118 = DIRECTION ( 'NONE',  ( -1.540237394707284220E-16, -1.793354297423764243E-16, 1.000000000000000000 ) ) ;
#7119 = CARTESIAN_POINT ( 'NONE',  ( 11.22215374030650281, 42.96218137147968008, 65.80574467885102763 ) ) ;
#7120 = ORIENTED_EDGE ( 'NONE', *, *, #9272, .F. ) ;
#7121 = DIRECTION ( 'NONE',  ( 1.110223024625156540E-16, 1.000000000000000000, 5.922860397471808077E-17 ) ) ;
#7122 = CARTESIAN_POINT ( 'NONE',  ( -4.755598089612432133, 42.34966066996389600, 95.05433879953096721 ) ) ;
#7123 = VECTOR ( 'NONE', #18887, 1000.000000000000227 ) ;
#7124 = CARTESIAN_POINT ( 'NONE',  ( 31.03948732994507864, 45.16218137147969003, 76.90433879953100416 ) ) ;
#7125 = AXIS2_PLACEMENT_3D ( 'NONE', #2435, #13710, #18182 ) ;
#7126 = CARTESIAN_POINT ( 'NONE',  ( 3.122153740306552905, 48.66551347115873227, 91.35183880294498238 ) ) ;
#7127 = CARTESIAN_POINT ( 'NONE',  ( -7.266087475274113139, 41.62398317295264860, 78.93401657524854897 ) ) ;
#7128 = CARTESIAN_POINT ( 'NONE',  ( -3.215335549418882444, 36.89651455478302466, 77.93013364623398331 ) ) ;
#7129 = CARTESIAN_POINT ( 'NONE',  ( -7.082284374571017338, 47.04405276229815769, 78.10358362899698648 ) ) ;
#7130 = CARTESIAN_POINT ( 'NONE',  ( 5.568489401881125289, 48.03437091500646261, 92.91433880123798872 ) ) ;
#7131 = AXIS2_PLACEMENT_3D ( 'NONE', #8372, #16562, #14754 ) ;
#7132 = AXIS2_PLACEMENT_3D ( 'NONE', #18427, #2571, #13528 ) ;
#7133 = CARTESIAN_POINT ( 'NONE',  ( 6.877103025211564358, 37.88742324339783352, 76.41040896618429201 ) ) ;
#7134 = ORIENTED_EDGE ( 'NONE', *, *, #1943, .T. ) ;
#7135 = DIRECTION ( 'NONE',  ( -1.110223024625156540E-16, -1.000000000000000000, -5.922860397471808077E-17 ) ) ;
#7136 = EDGE_LOOP ( 'NONE', ( #2207, #9929, #9442, #11011, #20480 ) ) ;
#7137 = VECTOR ( 'NONE', #12678, 1000.000000000000000 ) ;
#7138 = CARTESIAN_POINT ( 'NONE',  ( -4.777409764772176715, 51.19107953768585872, 78.82882669246485818 ) ) ;
#7139 = CARTESIAN_POINT ( 'NONE',  ( 6.198496396448986090, 45.68315280215533392, 92.83621380123798872 ) ) ;
#7140 = VERTEX_POINT ( 'NONE', #10752 ) ;
#7141 = LINE ( 'NONE', #8657, #12348 ) ;
#7142 = CARTESIAN_POINT ( 'NONE',  ( 29.77115333998617785, 40.36218137147969287, 105.5543387995310098 ) ) ;
#7143 = LINE ( 'NONE', #15563, #10875 ) ;
#7144 = CARTESIAN_POINT ( 'NONE',  ( -7.677846259693480668, 36.96218137147968008, 92.55433879953098142 ) ) ;
#7145 = CARTESIAN_POINT ( 'NONE',  ( 0.8488783891544954274, 52.96357957300006092, 76.31365475201417325 ) ) ;
#7146 = DIRECTION ( 'NONE',  ( 0.000000000000000000, 1.000000000000000000, 0.000000000000000000 ) ) ;
#7147 = ORIENTED_EDGE ( 'NONE', *, *, #19042, .T. ) ;
#7148 = VECTOR ( 'NONE', #14898, 1000.000000000000000 ) ;
#7149 = ADVANCED_FACE ( 'NONE', ( #6035 ), #4329, .T. ) ;
#7150 = CARTESIAN_POINT ( 'NONE',  ( 0.3869120917952209582, 35.96329670974013482, 78.57639762306027365 ) ) ;
#7151 = ORIENTED_EDGE ( 'NONE', *, *, #12651, .T. ) ;
#7152 = CARTESIAN_POINT ( 'NONE',  ( 2.522153740306508407, 50.16218137147969713, 66.55433879953099563 ) ) ;
#7153 = EDGE_CURVE ( 'NONE', #6140, #5774, #12536, .T. ) ;
#7154 = CARTESIAN_POINT ( 'NONE',  ( 6.961260622506120654, 50.34628710563859499, 76.69700829373513784 ) ) ;
#7155 = CARTESIAN_POINT ( 'NONE',  ( -1.219503646467429814, 49.90383875825364157, 53.41268141275706682 ) ) ;
#7156 = CARTESIAN_POINT ( 'NONE',  ( 0.5221537403065015237, 44.16218137147968292, 75.45433879953088763 ) ) ;
#7157 = CARTESIAN_POINT ( 'NONE',  ( 5.052198367669454626, 48.31320248322254685, 92.17308879782397923 ) ) ;
#7158 = CARTESIAN_POINT ( 'NONE',  ( -5.772695632942803634, 37.87151842650609268, 75.75097338717934292 ) ) ;
#7159 = EDGE_CURVE ( 'NONE', #445, #8755, #6036, .T. ) ;
#7160 = CARTESIAN_POINT ( 'NONE',  ( -4.230491984614289436, 51.58188695944873103, 75.39163409230444302 ) ) ;
#7161 = CARTESIAN_POINT ( 'NONE',  ( 5.146921702088428141, 37.39801444809555875, 77.71779572520892998 ) ) ;
#7162 = ORIENTED_EDGE ( 'NONE', *, *, #15267, .F. ) ;
#7163 = CARTESIAN_POINT ( 'NONE',  ( 8.790412360755956556, 41.13914800073450095, 78.76104738055306598 ) ) ;
#7164 = EDGE_CURVE ( 'NONE', #7741, #19935, #11340, .T. ) ;
#7165 = ORIENTED_EDGE ( 'NONE', *, *, #16004, .F. ) ;
#7166 = CARTESIAN_POINT ( 'NONE',  ( -4.307156007511903084, 51.52710565553512367, 75.38014013087713749 ) ) ;
#7167 = CARTESIAN_POINT ( 'NONE',  ( 4.987494971863720927, 47.58855820898865829, 92.21121379953100927 ) ) ;
#7168 = CARTESIAN_POINT ( 'NONE',  ( 3.122153740306552905, 48.66551347115873227, 94.78933879953099506 ) ) ;
#7169 = PRODUCT_DEFINITION_SHAPE ( 'NONE', 'NONE',  #21040 ) ;
#7170 = EDGE_LOOP ( 'NONE', ( #20841, #14542, #10169, #16391 ) ) ;
#7171 = CARTESIAN_POINT ( 'NONE',  ( 6.198496396448986090, 45.68315280215533392, 95.49246380123798872 ) ) ;
#7172 = CARTESIAN_POINT ( 'NONE',  ( 0.3333674555516544236, 52.96015614911942748, 77.71750738947619652 ) ) ;
#7173 = ORIENTED_EDGE ( 'NONE', *, *, #11209, .T. ) ;
#7174 = CARTESIAN_POINT ( 'NONE',  ( 5.378304226687590450, 36.81643649649897299, 75.37835156746757548 ) ) ;
#7175 = CARTESIAN_POINT ( 'NONE',  ( -6.341010505665811259, 41.98571378962061829, 78.93669174070734584 ) ) ;
#7176 = ORIENTED_EDGE ( 'NONE', *, *, #19619, .T. ) ;
#7177 = CARTESIAN_POINT ( 'NONE',  ( 2.113956822022224014, 52.20619733064047807, 78.36540345550628217 ) ) ;
#7178 = AXIS2_PLACEMENT_3D ( 'NONE', #8606, #15084, #498 ) ;
#7179 = ORIENTED_EDGE ( 'NONE', *, *, #18870, .T. ) ;
#7180 = CARTESIAN_POINT ( 'NONE',  ( -4.421065211396600247, 50.69879487670102236, 76.08363728426196815 ) ) ;
#7181 = CARTESIAN_POINT ( 'NONE',  ( 4.722153740306518799, 44.16218137147969003, 54.55433879953099563 ) ) ;
#7182 = AXIS2_PLACEMENT_3D ( 'NONE', #7105, #20085, #17015 ) ;
#7183 = CARTESIAN_POINT ( 'NONE',  ( -0.3080929418689875576, 37.85583172076933778, 91.19558880123798872 ) ) ;
#7184 = CONTEXT_DEPENDENT_SHAPE_REPRESENTATION ( #6670, #11944 ) ;
#7185 = CARTESIAN_POINT ( 'NONE',  ( -4.877877647307895970, 37.21055242598473001, 76.09452555557021469 ) ) ;
#7186 = ADVANCED_FACE ( 'NONE', ( #2538 ), #9738, .T. ) ;
#7187 = CARTESIAN_POINT ( 'NONE',  ( 0.3821786226492928651, 35.36301154328572949, 75.45433879953087342 ) ) ;
#7188 = CARTESIAN_POINT ( 'NONE',  ( 0.5221537403065008576, 44.16218137147969003, 105.5543387995310098 ) ) ;
#7189 = VERTEX_POINT ( 'NONE', #1052 ) ;
#7190 = CARTESIAN_POINT ( 'NONE',  ( 2.106328753683349042, 52.20158602024299910, 76.31288873172051979 ) ) ;
#7191 = EDGE_LOOP ( 'NONE', ( #8838, #387, #18907, #14194 ) ) ;
#7192 = CIRCLE ( 'NONE', #8916, 8.199999999999995737 ) ;
#7193 = CARTESIAN_POINT ( 'NONE',  ( 6.898851416363126710, 50.39238627222024292, 76.00796742194241062 ) ) ;
#7194 = CARTESIAN_POINT ( 'NONE',  ( 0.3284562911652677553, 52.35625317208734941, 77.72734411258261389 ) ) ;
#7195 = CARTESIAN_POINT ( 'NONE',  ( 2.043125170982144745, 38.48583871533720213, 95.17996380123798872 ) ) ;
#7196 = VECTOR ( 'NONE', #15644, 1000.000000000000000 ) ;
#7197 = VERTEX_POINT ( 'NONE', #8127 ) ;
#7198 = CARTESIAN_POINT ( 'NONE',  ( 6.487242172018640396, 49.78241043515765085, 78.48669174070734300 ) ) ;
#7199 = VERTEX_POINT ( 'NONE', #9035 ) ;
#7200 = LINE ( 'NONE', #20177, #2304 ) ;
#7201 = CARTESIAN_POINT ( 'NONE',  ( 5.599231707071657738, 51.35236299959863970, 78.30875056423674607 ) ) ;
#7202 = DIRECTION ( 'NONE',  ( -1.402518428993831676E-16, 1.000000000000000000, -0.000000000000000000 ) ) ;
#7203 = DIRECTION ( 'NONE',  ( -0.5941461771851691553, -0.8043570849667760481, -2.357623395011396791E-16 ) ) ;
#7204 = DIRECTION ( 'NONE',  ( -0.3165065846431824870, -0.9485903129789529098, 0.000000000000000000 ) ) ;
#7205 = DIRECTION ( 'NONE',  ( -0.5941461771851692664, -0.8043570849667761591, -2.357623395011396791E-16 ) ) ;
#7206 = CARTESIAN_POINT ( 'NONE',  ( 8.807466118993687587, 41.19025919604325026, 76.04813117819971069 ) ) ;
#7207 = CARTESIAN_POINT ( 'NONE',  ( -0.9988176903691428077, 49.83852402762217082, 91.89871380123798872 ) ) ;
#7209 = CARTESIAN_POINT ( 'NONE',  ( -6.779084170873278303, 43.37104029486602030, 76.06610350541322418 ) ) ;
#7208 = AXIS2_PLACEMENT_3D ( 'NONE', #16700, #6603, #7213 ) ;
#7210 = CARTESIAN_POINT ( 'NONE',  ( 5.270799808619019089, 50.67012946595514933, 75.36064185147203887 ) ) ;
#7211 = CARTESIAN_POINT ( 'NONE',  ( -2.077846259693550746, 39.65884927180063357, 93.22683880294496817 ) ) ;
#7212 = AXIS2_PLACEMENT_3D ( 'NONE', #16067, #3187, #20724 ) ;
#7213 = DIRECTION ( 'NONE',  ( 1.301042606982606060E-16, 1.000000000000000000, 0.000000000000000000 ) ) ;
#7214 = ORIENTED_EDGE ( 'NONE', *, *, #20510, .T. ) ;
#7215 = DIRECTION ( 'NONE',  ( -0.8136266022445296509, -0.5813877811925719508, -2.295812393977019367E-16 ) ) ;
#7216 = ORIENTED_EDGE ( 'NONE', *, *, #16509, .F. ) ;
#7217 = CARTESIAN_POINT ( 'NONE',  ( -4.664487479516252755, 37.05292970491732518, 75.97486526700035370 ) ) ;
#7218 = CARTESIAN_POINT ( 'NONE',  ( -3.767527516087995743, 38.37954780350102624, 75.97198585835440099 ) ) ;
#7219 = CARTESIAN_POINT ( 'NONE',  ( -4.181418169567056253, 51.61695331097443784, 79.50772166908967620 ) ) ;
#7220 = CARTESIAN_POINT ( 'NONE',  ( 2.043125170982144745, 38.48583871533720213, 93.92996380123798872 ) ) ;
#7221 = ADVANCED_FACE ( 'NONE', ( #935 ), #14025, .F. ) ;
#7222 = VECTOR ( 'NONE', #13875, 1000.000000000000114 ) ;
#7223 = CARTESIAN_POINT ( 'NONE',  ( -4.956093006374735488, 37.26832696102056275, 77.32892190166411694 ) ) ;
#7224 = LINE ( 'NONE', #10343, #4157 ) ;
#7225 = CARTESIAN_POINT ( 'NONE',  ( 0.3326973149608338787, 52.96014171822455552, 78.50066232894263862 ) ) ;
#7226 = VECTOR ( 'NONE', #5173, 1000.000000000000114 ) ;
#7227 = CARTESIAN_POINT ( 'NONE',  ( -2.077846259693550746, 39.65884927180063357, 93.22683880294496817 ) ) ;
#7228 = VERTEX_POINT ( 'NONE', #16534 ) ;
#7229 = ORIENTED_EDGE ( 'NONE', *, *, #12729, .F. ) ;
#7230 = CARTESIAN_POINT ( 'NONE',  ( 9.294532183588495755, 42.65002709052886587, 79.09515810002898206 ) ) ;
#7231 = CARTESIAN_POINT ( 'NONE',  ( -3.934466035114215554, 36.51369227099507242, 75.53057231289058393 ) ) ;
#7232 = LINE ( 'NONE', #1177, #9599 ) ;
#7233 = DIRECTION ( 'NONE',  ( 1.000000000000000000, -0.000000000000000000, -0.000000000000000000 ) ) ;
#7234 = DIRECTION ( 'NONE',  ( -3.211742425186504723E-16, 5.922860397471811774E-17, -1.000000000000000000 ) ) ;
#7235 = EDGE_CURVE ( 'NONE', #16996, #8020, #242, .T. ) ;
#7236 = CARTESIAN_POINT ( 'NONE',  ( -4.176309363623030180, 42.45208065485131499, 93.11058879611698558 ) ) ;
#7237 = CARTESIAN_POINT ( 'NONE',  ( 5.025485839985549319, 41.56218137147963887, 93.53933880294496817 ) ) ;
#7238 =( BOUNDED_CURVE ( )  B_SPLINE_CURVE ( 2, ( #11655, #18132, #16536 ),
 .UNSPECIFIED., .F., .F. ) 
 B_SPLINE_CURVE_WITH_KNOTS ( ( 3, 3 ),
 ( 0.2577596748367579904, 0.2583811345117278391 ),
 .UNSPECIFIED. ) 
 CURVE ( )  GEOMETRIC_REPRESENTATION_ITEM ( )  RATIONAL_B_SPLINE_CURVE ( ( 0.9674132986343859653, 0.9666957150223149942, 0.9660722070828959840 ) ) 
 REPRESENTATION_ITEM ( '' )  );
#7239 = CARTESIAN_POINT ( 'NONE',  ( 9.539487329945080418, 45.16218137147970424, 75.00433879953099847 ) ) ;
#7240 = AXIS2_PLACEMENT_3D ( 'NONE', #18732, #10353, #18835 ) ;
#7241 = CARTESIAN_POINT ( 'NONE',  ( -3.568560454108622881, 36.24341255788211669, 78.11242031084098869 ) ) ;
#7242 = CARTESIAN_POINT ( 'NONE',  ( -6.846424213726333363, 47.75094062703928444, 78.32492703482499508 ) ) ;
#7243 = CARTESIAN_POINT ( 'NONE',  ( 6.198496396448986090, 45.68315280215533392, 92.83621380123798872 ) ) ;
#7244 = CARTESIAN_POINT ( 'NONE',  ( -8.008709175654551871, 42.00064040251377406, 79.51261075138046408 ) ) ;
#7245 = CARTESIAN_POINT ( 'NONE',  ( 5.901490163600553451, 51.12909685347405286, 78.67852979887695142 ) ) ;
#7246 = CARTESIAN_POINT ( 'NONE',  ( 5.576345338833139209, 50.61463229589440260, 77.01219674908871582 ) ) ;
#7247 = VERTEX_POINT ( 'NONE', #6838 ) ;
#7248 = EDGE_CURVE ( 'NONE', #20516, #15383, #349, .T. ) ;
#7249 = CARTESIAN_POINT ( 'NONE',  ( -5.154188915835984375, 42.64120994080404614, 92.21121380123797451 ) ) ;
#7250 = VERTEX_POINT ( 'NONE', #13344 ) ;
#7251 = CARTESIAN_POINT ( 'NONE',  ( -5.616286711741430793, 44.43019146960381960, 93.89183879782397923 ) ) ;
#7252 = VECTOR ( 'NONE', #14413, 1000.000000000000000 ) ;
#7253 = CARTESIAN_POINT ( 'NONE',  ( 28.52215374030649997, 44.16218137147968292, 87.05433879953099563 ) ) ;
#7254 = CARTESIAN_POINT ( 'NONE',  ( -2.938659133435201465, 51.58520783560351930, 78.58955347608575437 ) ) ;
#7255 = CARTESIAN_POINT ( 'NONE',  ( 23.63948732994508006, 43.16218137147968292, 76.90433879953101837 ) ) ;
#7256 = CARTESIAN_POINT ( 'NONE',  ( 5.668901936282467524, 51.30090040776863702, 77.27261723006257910 ) ) ;
#7257 = CARTESIAN_POINT ( 'NONE',  ( -3.964734524320792541, 36.53605038468284505, 79.39152984579853012 ) ) ;
#7258 = ORIENTED_EDGE ( 'NONE', *, *, #9501, .F. ) ;
#7259 = CARTESIAN_POINT ( 'NONE',  ( 5.275862854764398868, 50.84374355665323719, 78.00102387806451532 ) ) ;
#7260 = EDGE_CURVE ( 'NONE', #11839, #10593, #16582, .T. ) ;
#7261 = VERTEX_POINT ( 'NONE', #14725 ) ;
#7262 = CARTESIAN_POINT ( 'NONE',  ( 30.92220646078100188, 45.56218137147968861, 56.80715055817104542 ) ) ;
#7263 = CARTESIAN_POINT ( 'NONE',  ( 23.03948732994508575, 43.16218137147968292, 77.50433879953099847 ) ) ;
#7264 = CARTESIAN_POINT ( 'NONE',  ( -7.157526761188767850, 41.72840140584739288, 76.21059579996631328 ) ) ;
#7265 = CARTESIAN_POINT ( 'NONE',  ( 5.760694563098077481, 51.23309689197249384, 79.54845644658969661 ) ) ;
#7266 = ADVANCED_FACE ( 'NONE', ( #16439 ), #2908, .F. ) ;
#7267 = LINE ( 'NONE', #12175, #1999 ) ;
#7268 = CARTESIAN_POINT ( 'NONE',  ( -1.419351766502868317, 49.49642391118513274, 93.65746379782397923 ) ) ;
#7269 = DIRECTION ( 'NONE',  ( -1.000000000000000000, 0.000000000000000000, -1.196361017915039239E-16 ) ) ;
#7270 = ORIENTED_EDGE ( 'NONE', *, *, #10429, .T. ) ;
#7271 = CARTESIAN_POINT ( 'NONE',  ( 8.221417502521635612, 41.35409244860189659, 78.83414475571305502 ) ) ;
#7272 = EDGE_CURVE ( 'NONE', #16704, #9302, #5651, .T. ) ;
#7273 = ADVANCED_FACE ( 'NONE', ( #782 ), #7368, .F. ) ;
#7274 = EDGE_CURVE ( 'NONE', #4353, #2902, #13860, .T. ) ;
#7275 = ORIENTED_EDGE ( 'NONE', *, *, #1526, .T. ) ;
#7276 = CARTESIAN_POINT ( 'NONE',  ( -4.477846259693498254, 37.66218137147969713, 54.55433879953098852 ) ) ;
#7277 = ADVANCED_FACE ( 'NONE', ( #20340 ), #989, .T. ) ;
#7278 = CARTESIAN_POINT ( 'NONE',  ( 5.025485839985549319, 41.56218137147963887, 93.22683879953099506 ) ) ;
#7279 = CARTESIAN_POINT ( 'NONE',  ( -7.895868156129457027, 41.57675978324414245, 77.84082762752957763 ) ) ;
#7280 = ORIENTED_EDGE ( 'NONE', *, *, #106, .F. ) ;
#7281 = CARTESIAN_POINT ( 'NONE',  ( 2.043125170982144745, 38.48583871533720213, 93.92996380123798872 ) ) ;
#7282 = CARTESIAN_POINT ( 'NONE',  ( 4.673174852049361228, 39.63213674411673537, 94.20433879782400766 ) ) ;
#7283 = DIRECTION ( 'NONE',  ( 0.8043570849667760481, -0.5941461771851693774, 1.733862608106482338E-17 ) ) ;
#7284 = ORIENTED_EDGE ( 'NONE', *, *, #20291, .T. ) ;
#7285 = B_SPLINE_CURVE_WITH_KNOTS ( 'NONE', 3,
 ( #5861, #12364, #10775, #1079, #7567, #5959, #18938, #8851, #3937, #10463, #16928, #2351, #5639, #12148, #6886, #8611 ),
 .UNSPECIFIED., .F., .F.,
 ( 4, 2, 2, 2, 2, 2, 2, 4 ),
 ( 0.000000000000000000, 0.0007059943671309979558, 0.0008824929589137576634, 0.001058991550696517263, 0.001411988734262035810, 0.001764985917827553924, 0.002117983101393071822, 0.002823977468524106749 ),
 .UNSPECIFIED. ) ;
#7286 = CARTESIAN_POINT ( 'NONE',  ( 23.03948732994508575, 45.16218137147969003, 77.50433879953099847 ) ) ;
#7287 = CARTESIAN_POINT ( 'NONE',  ( -4.796459876899764829, 51.17746702502860501, 78.71090438869831019 ) ) ;
#7288 = EDGE_CURVE ( 'NONE', #19085, #14373, #1636, .T. ) ;
#7289 = VERTEX_POINT ( 'NONE', #5451 ) ;
#7290 = CYLINDRICAL_SURFACE ( 'NONE', #9538, 4.200000000000000178 ) ;
#7291 = CARTESIAN_POINT ( 'NONE',  ( 6.828503391016846891, 43.33193468930419101, 94.16433880123797451 ) ) ;
#7292 = ORIENTED_EDGE ( 'NONE', *, *, #15156, .F. ) ;
#7293 = DIRECTION ( 'NONE',  ( 1.000000000000000000, -1.110223024625156540E-16, 1.779391786395883043E-16 ) ) ;
#7294 = DIRECTION ( 'NONE',  ( 0.7938652969193402686, -0.6080936526121349939, 1.322136515274840486E-17 ) ) ;
#7295 = PRODUCT_CONTEXT ( 'NONE', #7770, 'mechanical' ) ;
#7296 = CARTESIAN_POINT ( 'NONE',  ( -4.895593109503407980, 37.22363812428620378, 76.38448585835440952 ) ) ;
#7297 = DIRECTION ( 'NONE',  ( -1.000000000000000000, 0.000000000000000000, 0.000000000000000000 ) ) ;
#7298 = CARTESIAN_POINT ( 'NONE',  ( 9.271561067608034890, 45.68041113525027441, 79.47125056423675460 ) ) ;
#7299 = ORIENTED_EDGE ( 'NONE', *, *, #13409, .T. ) ;
#7300 = ORIENTED_EDGE ( 'NONE', *, *, #10312, .T. ) ;
#7301 = CARTESIAN_POINT ( 'NONE',  ( 2.094612936638713840, 52.20167840376603152, 76.22990676838142576 ) ) ;
#7302 = ORIENTED_EDGE ( 'NONE', *, *, #10844, .F. ) ;
#7303 = CARTESIAN_POINT ( 'NONE',  ( -0.6075024185379280794, 52.28440471269894374, 79.22274745980693922 ) ) ;
#7304 = ADVANCED_FACE ( 'NONE', ( #3962 ), #10486, .T. ) ;
#7305 = DIRECTION ( 'NONE',  ( -0.9999689119394086223, 0.007885122365275665235, -1.526048693634353392E-16 ) ) ;
#7306 = CARTESIAN_POINT ( 'NONE',  ( 6.198496396448986090, 45.68315280215533392, 92.99246380123798872 ) ) ;
#7307 = B_SPLINE_SURFACE_WITH_KNOTS ( 'NONE', 3, 1, ( 
 ( #9642, #12336 ),
 ( #7924, #16019 ),
 ( #14411, #15522 ),
 ( #19295, #6311 ),
 ( #12812, #8027 ),
 ( #20400, #9036 ),
 ( #20980, #10651 ),
 ( #6414, #19402 ),
 ( #18707, #4120 ),
 ( #11343, #9143 ),
 ( #5718, #20782 ),
 ( #4821, #937 ),
 ( #9740, #7424 ),
 ( #15632, #13918 ),
 ( #17812, #18818 ),
 ( #16221, #7320 ),
 ( #13809, #2539 ),
 ( #147, #8129 ),
 ( #6629, #350 ),
 ( #8557, #17913 ),
 ( #13032, #11441 ),
 ( #4920, #14621 ),
 ( #6839, #13130 ) ),
 .UNSPECIFIED., .F., .F., .F.,
 ( 4, 1, 1, 1, 1, 1, 1, 1, 1, 1, 1, 1, 1, 1, 1, 1, 1, 1, 1, 1, 4 ),
 ( 2, 2 ),
 ( 0.000000000000000000, 0.04683093660151300269, 0.09055667580802433114, 0.1312013806050136844, 0.1681729499244319359, 0.2024082766003676426, 0.2330515569695218725, 0.2607881417524846590, 0.2857054801288026469, 0.3326652789510584074, 0.3814982805224741425, 0.4333318279156733732, 0.4889629060548432160, 0.5467408684218817427, 0.6046224851005120859, 0.6645427963802341687, 0.7261481924644412889, 0.7902890061914499276, 0.8570127982043956871, 0.9269126820953633716, 1.000000000000000000 ),
 ( 0.000000000000000000, 1.000000000000000000 ),
 .UNSPECIFIED. ) ;
#7308 = ORIENTED_EDGE ( 'NONE', *, *, #17478, .F. ) ;
#7309 = ADVANCED_FACE ( 'NONE', ( #8880 ), #15367, .F. ) ;
#7310 = PLANE ( 'NONE',  #18452 ) ;
#7311 = EDGE_LOOP ( 'NONE', ( #7292, #3914, #4590, #11791 ) ) ;
#7312 = DIRECTION ( 'NONE',  ( -0.5813877811927012917, 0.8136266022444372803, 5.636455622144620416E-17 ) ) ;
#7313 = DIRECTION ( 'NONE',  ( 0.8136266022444427204, 0.5813877811926937422, 2.295812393977104662E-16 ) ) ;
#7314 = CARTESIAN_POINT ( 'NONE',  ( 7.677801029594266247, 40.18576601801834869, 76.30598982719874357 ) ) ;
#7315 = CARTESIAN_POINT ( 'NONE',  ( 5.611423337425062385, 41.22389019960463230, 92.67996380123805977 ) ) ;
#7316 = CARTESIAN_POINT ( 'NONE',  ( -3.805620430632945528, 51.12781903265568673, 79.50514382629147292 ) ) ;
#7317 = CARTESIAN_POINT ( 'NONE',  ( -0.9388773962491546721, 52.84004908296358138, 77.21536821129558348 ) ) ;
#7318 = CARTESIAN_POINT ( 'NONE',  ( 2.043125170982144745, 38.48583871533720213, 95.17996380123798872 ) ) ;
#7319 = CARTESIAN_POINT ( 'NONE',  ( 8.255193350648697859, 41.45511835277029178, 75.98994273744924044 ) ) ;
#7320 = CARTESIAN_POINT ( 'NONE',  ( -4.952713483362852109, 50.14603833638137331, 75.54244301425877950 ) ) ;
#7321 = CARTESIAN_POINT ( 'NONE',  ( 3.122153740306552905, 48.66551347115873227, 91.35183880294498238 ) ) ;
#7322 = B_SPLINE_CURVE_WITH_KNOTS ( 'NONE', 3,
 ( #11644, #8335, #18122, #19393, #13022, #8229, #11535, #11331, #19496, #17803, #6830, #3227, #3433, #13336, #14816, #1532, #9832, #19809, #14717, #16110, #20971, #9730, #235, #1637, #137, #13121 ),
 .UNSPECIFIED., .F., .F.,
 ( 4, 2, 2, 2, 2, 2, 2, 2, 2, 2, 2, 2, 4 ),
 ( 0.000000000000000000, 0.001352842588461793333, 0.002029263882692689241, 0.002705685176923584932, 0.004058527765385377614, 0.004734949059616283713, 0.005411370353847190680, 0.006764212942309022827, 0.007440634236539929794, 0.008117055530770836760, 0.008793476825001741992, 0.009469898119232647224, 0.01082274070769447677 ),
 .UNSPECIFIED. ) ;
#7323 = LINE ( 'NONE', #13812, #4141 ) ;
#7324 = VERTEX_POINT ( 'NONE', #13973 ) ;
#7325 = CARTESIAN_POINT ( 'NONE',  ( 8.949064546045571333, 41.61463866475444462, 78.77153038569251464 ) ) ;
#7326 = ORIENTED_EDGE ( 'NONE', *, *, #1954, .F. ) ;
#7327 = CARTESIAN_POINT ( 'NONE',  ( 8.722153740306483272, 51.36218137147968577, 95.05433879953098142 ) ) ;
#7328 = CARTESIAN_POINT ( 'NONE',  ( 4.134898411747151670, 47.90306806511021875, 95.05422504033560926 ) ) ;
#7329 = CARTESIAN_POINT ( 'NONE',  ( 0.5221537403065050764, 50.16218137147969713, 85.15433879953098995 ) ) ;
#7330 = CARTESIAN_POINT ( 'NONE',  ( -5.154188915835984375, 42.64120994080404614, 94.86746380123797451 ) ) ;
#7331 = LINE ( 'NONE', #20195, #2064 ) ;
#7332 = CARTESIAN_POINT ( 'NONE',  ( -8.312169971356507148, 42.89858049018356212, 78.28007409364852265 ) ) ;
#7333 = CARTESIAN_POINT ( 'NONE',  ( -0.1994209430448784792, 35.36759766960258844, 76.86610350541323555 ) ) ;
#7334 = DIRECTION ( 'NONE',  ( 0.007885122365275663500, 0.9999689119394085113, 1.805443505845543142E-16 ) ) ;
#7335 = ORIENTED_EDGE ( 'NONE', *, *, #10629, .T. ) ;
#7336 = VERTEX_POINT ( 'NONE', #20017 ) ;
#7337 = CARTESIAN_POINT ( 'NONE',  ( 9.307108147255313213, 42.68771805144258735, 79.03485483908291087 ) ) ;
#7338 = CARTESIAN_POINT ( 'NONE',  ( 5.665287683258889651, 37.02150436742986273, 75.36022115247205022 ) ) ;
#7339 = LINE ( 'NONE', #5740, #3813 ) ;
#7340 = CARTESIAN_POINT ( 'NONE',  ( 5.924340528221679669, 51.11221820959726614, 77.13671500005938242 ) ) ;
#7341 = CARTESIAN_POINT ( 'NONE',  ( -2.931538964508604739, 39.51556981890902165, 95.05433879953095300 ) ) ;
#7342 = CARTESIAN_POINT ( 'NONE',  ( 8.445623910622046537, 42.47021319322472976, 78.07975471416389723 ) ) ;
#7343 = CARTESIAN_POINT ( 'NONE',  ( 1.256812508749381774, 49.74246873332880625, 91.42996380294499659 ) ) ;
#7344 = CARTESIAN_POINT ( 'NONE',  ( -4.383574773872678243, 51.47249960296332461, 76.44257241107362688 ) ) ;
#7345 = CARTESIAN_POINT ( 'NONE',  ( -7.727380346712589443, 47.23718031655728566, 77.58227997600145898 ) ) ;
#7346 = CARTESIAN_POINT ( 'NONE',  ( -0.9988176903691428077, 49.83852402762217082, 90.64871380123798872 ) ) ;
#7347 = PRODUCT_DEFINITION_SHAPE ( 'NONE', 'NONE',  #21036 ) ;
#7348 = CARTESIAN_POINT ( 'NONE',  ( 6.582016959483238949, 37.67656554461878926, 75.62429547252081363 ) ) ;
#7349 = ORIENTED_EDGE ( 'NONE', *, *, #17420, .T. ) ;
#7350 = CARTESIAN_POINT ( 'NONE',  ( 5.916041096196198446, 51.11834866571297908, 77.16780247135808679 ) ) ;
#7351 = ORIENTED_EDGE ( 'NONE', *, *, #13418, .F. ) ;
#7352 = CARTESIAN_POINT ( 'NONE',  ( -4.413575733319255789, 50.70414658352780179, 78.86176377286571437 ) ) ;
#7353 =( REPRESENTATION_RELATIONSHIP ('NONE','NONE', #11365, #7678 ) REPRESENTATION_RELATIONSHIP_WITH_TRANSFORMATION ( #15713 )SHAPE_REPRESENTATION_RELATIONSHIP( ) );
#7354 = CARTESIAN_POINT ( 'NONE',  ( 6.198496396448986090, 45.68315280215533392, 90.33621380123798872 ) ) ;
#7355 = ORIENTED_EDGE ( 'NONE', *, *, #14780, .T. ) ;
#7356 = FACE_OUTER_BOUND ( 'NONE', #18105, .T. ) ;
#7357 = CARTESIAN_POINT ( 'NONE',  ( -0.8111795930268322907, 49.49551470481303994, 61.82100546619766845 ) ) ;
#7358 = VECTOR ( 'NONE', #4540, 1000.000000000000000 ) ;
#7359 = CARTESIAN_POINT ( 'NONE',  ( -2.920516602815223184, 51.59817182374411715, 78.36353918055804968 ) ) ;
#7360 = LINE ( 'NONE', #17157, #8078 ) ;
#7361 = CARTESIAN_POINT ( 'NONE',  ( 5.571366797620176392, 51.37294568574342435, 77.09285305542944400 ) ) ;
#7362 = CYLINDRICAL_SURFACE ( 'NONE', #17071, 3.999999999999996447 ) ;
#7363 = ORIENTED_EDGE ( 'NONE', *, *, #8965, .T. ) ;
#7364 = CARTESIAN_POINT ( 'NONE',  ( 6.457023732898393042, 39.40536329938229443, 75.45433879953087342 ) ) ;
#7365 = VERTEX_POINT ( 'NONE', #8984 ) ;
#7366 = LINE ( 'NONE', #17371, #4019 ) ;
#7367 = DIRECTION ( 'NONE',  ( -0.5813877811927011807, 0.8136266022444372803, 5.636455622144619183E-17 ) ) ;
#7368 = PLANE ( 'NONE',  #12846 ) ;
#7369 = ADVANCED_FACE ( 'NONE', ( #10704 ), #17267, .F. ) ;
#7370 = B_SPLINE_CURVE_WITH_KNOTS ( 'NONE', 3,
 ( #17742, #13166, #4956, #3174, #8275, #19435, #179, #11581, #11375, #17846, #3269, #19639 ),
 .UNSPECIFIED., .F., .F.,
 ( 4, 2, 2, 2, 2, 4 ),
 ( 0.000000000000000000, 0.0001366260637585213467, 0.0002049390956377732380, 0.0002732521275170251293, 0.0004098781912754880376, 0.0005465042550339509458 ),
 .UNSPECIFIED. ) ;
#7371 = CARTESIAN_POINT ( 'NONE',  ( -7.308728793983235938, 40.14750922464471472, 78.21036603407506504 ) ) ;
#7372 = PLANE ( 'NONE',  #16264 ) ;
#7373 = CARTESIAN_POINT ( 'NONE',  ( 6.660594192354429843, 43.89417127335556046, 94.51683879782399345 ) ) ;
#7374 = CARTESIAN_POINT ( 'NONE',  ( 6.488325228803680567, 49.78755270998220084, 78.57237519692213823 ) ) ;
#7375 = PRESENTATION_LAYER_ASSIGNMENT (  '', '', ( #12472 ) ) ;
#7376 = VERTEX_POINT ( 'NONE', #15467 ) ;
#7377 = CARTESIAN_POINT ( 'NONE',  ( 4.574454570626803829, 51.29112378112938586, 77.67115886575356853 ) ) ;
#7378 = ORIENTED_EDGE ( 'NONE', *, *, #19135, .F. ) ;
#7379 = FACE_OUTER_BOUND ( 'NONE', #1844, .T. ) ;
#7380 = EDGE_CURVE ( 'NONE', #5156, #13025, #5777, .T. ) ;
#7381 = CARTESIAN_POINT ( 'NONE',  ( 5.544968037009670780, 45.50804040601273925, 92.13308879953099506 ) ) ;
#7382 = CARTESIAN_POINT ( 'NONE',  ( -8.036666733872158019, 42.02200910348221186, 77.21863129581211638 ) ) ;
#7383 = EDGE_LOOP ( 'NONE', ( #16554, #19330, #15299, #17876 ) ) ;
#7384 = CARTESIAN_POINT ( 'NONE',  ( 5.568489401881125289, 48.03437091500646261, 93.07058880123797451 ) ) ;
#7385 = CARTESIAN_POINT ( 'NONE',  ( -5.616286711741430793, 44.43019146960381960, 94.98558879782399345 ) ) ;
#7386 = CARTESIAN_POINT ( 'NONE',  ( 0.3442881027912784719, 52.96038515679411773, 77.58553688243358692 ) ) ;
#7387 = AXIS2_PLACEMENT_3D ( 'NONE', #5830, #15739, #12334 ) ;
#7388 = FACE_OUTER_BOUND ( 'NONE', #1040, .T. ) ;
#7389 = CARTESIAN_POINT ( 'NONE',  ( 2.522153740306498193, 49.81903562097208038, 123.5543387995310098 ) ) ;
#7390 = EDGE_CURVE ( 'NONE', #500, #11984, #18863, .T. ) ;
#7391 = ORIENTED_EDGE ( 'NONE', *, *, #16848, .T. ) ;
#7392 = DIRECTION ( 'NONE',  ( -0.000000000000000000, -0.000000000000000000, 1.000000000000000000 ) ) ;
#7393 = CARTESIAN_POINT ( 'NONE',  ( 0.7788067644200915574, 52.35270196965525002, 78.85266037376247539 ) ) ;
#7394 = AXIS2_PLACEMENT_3D ( 'NONE', #17625, #14907, #332 ) ;
#7395 = ORIENTED_EDGE ( 'NONE', *, *, #4396, .F. ) ;
#7396 = CARTESIAN_POINT ( 'NONE',  ( 11.22215374030650281, 42.96218137147968008, 65.80574467885102763 ) ) ;
#7397 = CARTESIAN_POINT ( 'NONE',  ( -1.219503646467433144, 49.90383875825363447, 85.41268141275706682 ) ) ;
#7398 = EDGE_CURVE ( 'NONE', #9413, #15226, #10799, .T. ) ;
#7399 = SHAPE_DEFINITION_REPRESENTATION ( #18037, #209 ) ;
#7400 = CARTESIAN_POINT ( 'NONE',  ( -4.804644443005473775, 51.17161863374555963, 78.45066232894264147 ) ) ;
#7401 = CARTESIAN_POINT ( 'NONE',  ( 5.431844598077052666, 36.85469448565577011, 76.44059830477070250 ) ) ;
#7402 = AXIS2_PLACEMENT_3D ( 'NONE', #14620, #18021, #1758 ) ;
#7403 = CARTESIAN_POINT ( 'NONE',  ( -7.221822550567737586, 41.46565244290277263, 78.36256670375607314 ) ) ;
#7404 = ORIENTED_EDGE ( 'NONE', *, *, #3244, .F. ) ;
#7405 = EDGE_CURVE ( 'NONE', #3900, #17868, #19169, .T. ) ;
#7406 = CARTESIAN_POINT ( 'NONE',  ( 1.561428751595478115, 52.95872086824613945, 75.52862058684291924 ) ) ;
#7407 = ORIENTED_EDGE ( 'NONE', *, *, #4434, .F. ) ;
#7408 = PLANE ( 'NONE',  #7461 ) ;
#7409 = DIRECTION ( 'NONE',  ( 1.540237394707284467E-16, 1.793354297423764243E-16, -1.000000000000000000 ) ) ;
#7410 = CARTESIAN_POINT ( 'NONE',  ( -5.784195910403845176, 44.99242805365518194, 92.28933880123798872 ) ) ;
#7411 = ORIENTED_EDGE ( 'NONE', *, *, #20873, .T. ) ;
#7412 = CARTESIAN_POINT ( 'NONE',  ( 11.22215374030649926, 42.76218137147968434, 69.40574467885102194 ) ) ;
#7413 = ORIENTED_EDGE ( 'NONE', *, *, #10710, .F. ) ;
#7414 = DIRECTION ( 'NONE',  ( -1.110223024625156540E-16, -1.000000000000000000, -5.922860397471808077E-17 ) ) ;
#7415 = FACE_OUTER_BOUND ( 'NONE', #18682, .T. ) ;
#7416 = CARTESIAN_POINT ( 'NONE',  ( 7.672101664393531806, 40.16868465895075957, 76.70090004521539129 ) ) ;
#7417 = VECTOR ( 'NONE', #16456, 1000.000000000000227 ) ;
#7418 = LINE ( 'NONE', #10748, #7358 ) ;
#7419 = CARTESIAN_POINT ( 'NONE',  ( -7.486598725001505805, 40.28313368935070571, 79.09912640779528203 ) ) ;
#7420 = FACE_OUTER_BOUND ( 'NONE', #13797, .T. ) ;
#7421 = DIRECTION ( 'NONE',  ( 0.000000000000000000, -1.000000000000000000, 0.000000000000000000 ) ) ;
#7422 = DIRECTION ( 'NONE',  ( 0.3165065846431826535, 0.9485903129789529098, 2.188653791613874008E-16 ) ) ;
#7423 = ADVANCED_FACE ( 'NONE', ( #17573 ), #4377, .F. ) ;
#7424 = CARTESIAN_POINT ( 'NONE',  ( -5.209532200270762914, 49.96252508401233428, 75.79002994479621691 ) ) ;
#7425 = CARTESIAN_POINT ( 'NONE',  ( 5.159368991072407873, 51.67727186915629289, 75.44114465464750197 ) ) ;
#7426 = EDGE_CURVE ( 'NONE', #5649, #18616, #12786, .T. ) ;
#7427 = CARTESIAN_POINT ( 'NONE',  ( -5.058133621542618030, 44.89684013992257405, 91.74246380294499659 ) ) ;
#7428 = CARTESIAN_POINT ( 'NONE',  ( -3.539401246598059991, 43.09270903039240608, 79.40903933791013003 ) ) ;
#7429 = EDGE_LOOP ( 'NONE', ( #5024, #14521, #10473, #1431 ) ) ;
#7430 = EDGE_CURVE ( 'NONE', #8992, #4353, #14203, .T. ) ;
#7431 = CARTESIAN_POINT ( 'NONE',  ( 8.898741081898894123, 41.46381605024582484, 78.92561463894257656 ) ) ;
#7432 = VECTOR ( 'NONE', #5971, 1000.000000000000000 ) ;
#7433 = EDGE_CURVE ( 'NONE', #13846, #12245, #17678, .T. ) ;
#7434 = VERTEX_POINT ( 'NONE', #14168 ) ;
#7435 = DIRECTION ( 'NONE',  ( 0.8136266022444372803, 0.5813877811927012917, 2.295812393977109100E-16 ) ) ;
#7436 = CARTESIAN_POINT ( 'NONE',  ( 10.77494014480653561, 42.96218137147968008, 77.80433879953099563 ) ) ;
#7437 = LINE ( 'NONE', #13930, #10943 ) ;
#7438 =( NAMED_UNIT ( * ) SI_UNIT ( $, .STERADIAN. ) SOLID_ANGLE_UNIT ( ) );
#7439 = EDGE_CURVE ( 'NONE', #9222, #8755, #6285, .T. ) ;
#7440 = CARTESIAN_POINT ( 'NONE',  ( -4.770044440429786370, 37.13090037985040226, 77.30667006270941499 ) ) ;
#7441 = CARTESIAN_POINT ( 'NONE',  ( -8.133968313267025962, 42.33505088355195056, 79.40422342893963048 ) ) ;
#7442 = FACE_OUTER_BOUND ( 'NONE', #18504, .T. ) ;
#7443 = ORIENTED_EDGE ( 'NONE', *, *, #848, .T. ) ;
#7444 = CARTESIAN_POINT ( 'NONE',  ( 0.5759855363013707263, 51.36198072897979472, 78.93669174070734584 ) ) ;
#7445 = CARTESIAN_POINT ( 'NONE',  ( 28.52215374030649997, 44.16218137147968292, 45.55433879953098852 ) ) ;
#7446 = CARTESIAN_POINT ( 'NONE',  ( 3.357643116058062649, 37.76218137147968434, 92.03489701350649455 ) ) ;
#7447 = DIRECTION ( 'NONE',  ( -1.779391786395883536E-16, -5.922860397471806844E-17, 1.000000000000000000 ) ) ;
#7448 = CARTESIAN_POINT ( 'NONE',  ( 8.951509595531131680, 41.62196663317372725, 77.18036020728871449 ) ) ;
#7449 = VECTOR ( 'NONE', #5126, 1000.000000000000000 ) ;
#7450 = CARTESIAN_POINT ( 'NONE',  ( 9.026838159693452823, 41.84773111872319618, 78.13669174070733447 ) ) ;
#7451 = CARTESIAN_POINT ( 'NONE',  ( -0.2125050281363792815, 38.58189400963055959, 90.80496380294498238 ) ) ;
#7452 = LINE ( 'NONE', #14049, #8112 ) ;
#7453 = VECTOR ( 'NONE', #5492, 1000.000000000000000 ) ;
#7454 = FACE_OUTER_BOUND ( 'NONE', #15779, .T. ) ;
#7455 = ADVANCED_FACE ( 'NONE', ( #14076 ), #2091, .T. ) ;
#7456 = CARTESIAN_POINT ( 'NONE',  ( 1.352400422481993658, 50.46853102219002096, 90.57058880123798872 ) ) ;
#7457 = VECTOR ( 'NONE', #6755, 1000.000000000000000 ) ;
#7458 = CARTESIAN_POINT ( 'NONE',  ( 5.833066520072705430, 37.14139298144173296, 75.36337631951366234 ) ) ;
#7459 = ORIENTED_EDGE ( 'NONE', *, *, #18091, .T. ) ;
#7460 = DIRECTION ( 'NONE',  ( -0.000000000000000000, -0.000000000000000000, 1.000000000000000000 ) ) ;
#7461 = AXIS2_PLACEMENT_3D ( 'NONE', #17303, #7520, #18688 ) ;
#7462 = ORIENTED_EDGE ( 'NONE', *, *, #19641, .T. ) ;
#7463 = LINE ( 'NONE', #18533, #12587 ) ;
#7464 = CARTESIAN_POINT ( 'NONE',  ( 1.256812508749381774, 49.74246873332880625, 92.67996380294498238 ) ) ;
#7465 = ORIENTED_EDGE ( 'NONE', *, *, #20418, .T. ) ;
#7466 = CARTESIAN_POINT ( 'NONE',  ( -1.306251101200015086, 49.87752504164859602, 77.32593395802449265 ) ) ;
#7468 = VECTOR ( 'NONE', #20553, 1000.000000000000000 ) ;
#7467 = CARTESIAN_POINT ( 'NONE',  ( -0.5342115424629445553, 52.21627705124925711, 75.64626500862765113 ) ) ;
#7469 = CLOSED_SHELL ( 'NONE', ( #18775, #9662, #20790, #3773, #15194, #2110, #16979, #15050, #16410, #6244, #9879, #12395, #13302, #1516, #6012, #19383, #19861 ) ) ;
#7470 = DIRECTION ( 'NONE',  ( -0.000000000000000000, -0.000000000000000000, 1.000000000000000000 ) ) ;
#7471 = CARTESIAN_POINT ( 'NONE',  ( 0.7902174608934043887, 52.95811370980002408, 77.46569632448046150 ) ) ;
#7472 = CARTESIAN_POINT ( 'NONE',  ( 14.52215374030650175, 40.36218137147969287, 105.5543387995309956 ) ) ;
#7473 = DIRECTION ( 'NONE',  ( -1.000000000000000000, 0.000000000000000000, 0.000000000000000000 ) ) ;
#7474 = ORIENTED_EDGE ( 'NONE', *, *, #15156, .T. ) ;
#7475 = CARTESIAN_POINT ( 'NONE',  ( 4.033749877938553219, 36.75212424151919777, 78.77947436490163113 ) ) ;
#7476 = CARTESIAN_POINT ( 'NONE',  ( 0.7901638384306278740, 50.30062182352762079, 93.42308879782399345 ) ) ;
#7477 = ORIENTED_EDGE ( 'NONE', *, *, #20414, .T. ) ;
#7478 = CARTESIAN_POINT ( 'NONE',  ( -3.729174670837895889, 37.14778277730540168, 75.44287404548305176 ) ) ;
#7479 = DIRECTION ( 'NONE',  ( 1.540237394707284220E-16, 1.793354297423764243E-16, -1.000000000000000000 ) ) ;
#7480 = VECTOR ( 'NONE', #16925, 1000.000000000000227 ) ;
#7481 = VECTOR ( 'NONE', #17174, 1000.000000000000000 ) ;
#7482 = CARTESIAN_POINT ( 'NONE',  ( 2.263363662449363822, 49.77488197367694767, 93.19231768333818877 ) ) ;
#7483 = LINE ( 'NONE', #14169, #3523 ) ;
#7484 = PLANE ( 'NONE',  #4690 ) ;
#7485 = CARTESIAN_POINT ( 'NONE',  ( 5.670718203856349504, 37.02538481862475805, 75.97247164366282846 ) ) ;
#7486 = CARTESIAN_POINT ( 'NONE',  ( 5.674841441279768084, 50.54324618507919809, 79.53726082601099279 ) ) ;
#7487 = B_SPLINE_SURFACE_WITH_KNOTS ( 'NONE', 3, 1, ( 
 ( #9900, #6676 ),
 ( #16379, #13182 ),
 ( #19656, #11599 ),
 ( #6786, #18177 ),
 ( #18074, #3593 ),
 ( #10102, #16585 ),
 ( #2005, #5507 ),
 ( #610, #7090 ),
 ( #5611, #20281 ),
 ( #10645, #10531 ),
 ( #12020, #18275 ),
 ( #8614, #17000 ),
 ( #10324, #16796 ),
 ( #17113, #2213 ),
 ( #15196, #404 ) ),
 .UNSPECIFIED., .F., .F., .F.,
 ( 4, 1, 1, 1, 1, 1, 1, 1, 1, 1, 1, 1, 4 ),
 ( 2, 2 ),
 ( 0.000000000000000000, 0.1027118292588455328, 0.1981555131143932502, 0.2874887429483043433, 0.3729525961046017413, 0.4183424594053214429, 0.4719402630404010424, 0.5343443080544488799, 0.6066182697135418245, 0.6887512500569755725, 0.7816623524051020677, 0.8855466611608181493, 1.000000000000000000 ),
 ( 0.000000000000000000, 1.000000000000000000 ),
 .UNSPECIFIED. ) ;
#7488 = VECTOR ( 'NONE', #11445, 1000.000000000000000 ) ;
#7489 = AXIS2_PLACEMENT_3D ( 'NONE', #8045, #20997, #12732 ) ;
#7490 = ORIENTED_EDGE ( 'NONE', *, *, #12747, .F. ) ;
#7491 = CARTESIAN_POINT ( 'NONE',  ( 8.851169967151880869, 41.32124240149376249, 78.93505401271374922 ) ) ;
#7492 = ORIENTED_EDGE ( 'NONE', *, *, #2723, .F. ) ;
#7493 = DIRECTION ( 'NONE',  ( 6.308085367188358884E-15, 0.000000000000000000, 1.000000000000000000 ) ) ;
#7494 = CARTESIAN_POINT ( 'NONE',  ( -5.784195910403845176, 44.99242805365518194, 94.78933880123798872 ) ) ;
#7495 =( GEOMETRIC_REPRESENTATION_CONTEXT ( 3 ) GLOBAL_UNCERTAINTY_ASSIGNED_CONTEXT ( ( #18728 ) ) GLOBAL_UNIT_ASSIGNED_CONTEXT ( ( #5370, #3676, #16465 ) ) REPRESENTATION_CONTEXT ( 'NONE', 'WORKASPACE' ) );
#7496 =( BOUNDED_CURVE ( )  B_SPLINE_CURVE ( 3, ( #9264, #12344, #15847, #10546 ),
 .UNSPECIFIED., .F., .F. ) 
 B_SPLINE_CURVE_WITH_KNOTS ( ( 4, 4 ),
 ( 1.982313172862386397, 2.094395102393197927 ),
 .UNSPECIFIED. ) 
 CURVE ( )  GEOMETRIC_REPRESENTATION_ITEM ( )  RATIONAL_B_SPLINE_CURVE ( ( 1.000000000000000000, 0.9989534107080366709, 0.9989534107080366709, 1.000000000000000000 ) ) 
 REPRESENTATION_ITEM ( '' )  );
#7497 = VERTEX_POINT ( 'NONE', #20313 ) ;
#7498 = EDGE_CURVE ( 'NONE', #5789, #16992, #8436, .T. ) ;
#7499 = CARTESIAN_POINT ( 'NONE',  ( 6.828503391016846891, 43.33193468930419101, 91.66433880123796030 ) ) ;
#7500 = FACE_OUTER_BOUND ( 'NONE', #8320, .T. ) ;
#7501 = FACE_OUTER_BOUND ( 'NONE', #9131, .T. ) ;
#7502 = CARTESIAN_POINT ( 'NONE',  ( 6.012275498921958672, 37.26944915646792822, 78.37198585835440667 ) ) ;
#7503 = FACE_OUTER_BOUND ( 'NONE', #8539, .T. ) ;
#7504 = ORIENTED_EDGE ( 'NONE', *, *, #1467, .T. ) ;
#7505 = CARTESIAN_POINT ( 'NONE',  ( 11.22215374030649926, 42.76218137147968434, 80.55433879953099563 ) ) ;
#7506 = CARTESIAN_POINT ( 'NONE',  ( 6.198496396448986090, 45.68315280215533392, 92.99246380123798872 ) ) ;
#7507 = VECTOR ( 'NONE', #17976, 1000.000000000000000 ) ;
#7508 = ORIENTED_EDGE ( 'NONE', *, *, #1990, .F. ) ;
#7509 = CARTESIAN_POINT ( 'NONE',  ( -5.044287576081563529, 45.27497882680665242, 92.45433879953097289 ) ) ;
#7510 = CARTESIAN_POINT ( 'NONE',  ( 2.263811127080453733, 49.90383875825364157, 61.41268141275705972 ) ) ;
#7511 = CARTESIAN_POINT ( 'NONE',  ( 1.352400422481993658, 50.46853102219002096, 90.57058880123798872 ) ) ;
#7512 = EDGE_CURVE ( 'NONE', #5268, #2768, #15339, .T. ) ;
#7513 = CARTESIAN_POINT ( 'NONE',  ( -1.477846259693491149, 49.16218137147969003, 58.55433879953100984 ) ) ;
#7514 = EDGE_CURVE ( 'NONE', #14664, #9181, #2314, .T. ) ;
#7515 = CARTESIAN_POINT ( 'NONE',  ( 5.427951760950261217, 36.85191280677083370, 76.67247627436783830 ) ) ;
#7516 = CARTESIAN_POINT ( 'NONE',  ( 0.5221537403065005245, 44.16218137147968292, 82.45433879953087342 ) ) ;
#7517 = VERTEX_POINT ( 'NONE', #12766 ) ;
#7518 = CARTESIAN_POINT ( 'NONE',  ( 1.826366013274308475, 52.20379362933912404, 75.70482343270806780 ) ) ;
#7519 = ORIENTED_EDGE ( 'NONE', *, *, #16848, .F. ) ;
#7520 = DIRECTION ( 'NONE',  ( 0.7071067811865539010, -3.662367542345418158E-17, -0.7071067811865411334 ) ) ;
#7521 = CARTESIAN_POINT ( 'NONE',  ( -3.154801521863568325, 47.83913663364971569, 92.55433879953098142 ) ) ;
#7522 = CARTESIAN_POINT ( 'NONE',  ( -0.3080929418689875576, 37.85583172076933778, 91.35183880123798872 ) ) ;
#7523 = ORIENTED_EDGE ( 'NONE', *, *, #6448, .F. ) ;
#7524 = ORIENTED_EDGE ( 'NONE', *, *, #12338, .T. ) ;
#7525 = CARTESIAN_POINT ( 'NONE',  ( -4.616093716651582746, 50.55342697692977083, 75.38579245895105885 ) ) ;
#7526 = VECTOR ( 'NONE', #18632, 1000.000000000000000 ) ;
#7527 = ORIENTED_EDGE ( 'NONE', *, *, #15477, .T. ) ;
#7528 = CARTESIAN_POINT ( 'NONE',  ( 4.239508620224502700, 51.44272066563755175, 79.02133806855546538 ) ) ;
#7529 = CARTESIAN_POINT ( 'NONE',  ( 1.215246153217547365, 50.28109722957945138, 51.67325465763073566 ) ) ;
#7530 = CARTESIAN_POINT ( 'NONE',  ( 7.670823270696295104, 40.16485323194035573, 77.08252479744105301 ) ) ;
#7531 = VERTEX_POINT ( 'NONE', #12558 ) ;
#7532 = CARTESIAN_POINT ( 'NONE',  ( 6.436008563395697379, 49.84285157267152755, 75.88622433235630638 ) ) ;
#7533 = CARTESIAN_POINT ( 'NONE',  ( -7.782852850910068732, 41.21998227328707287, 79.53187240040659844 ) ) ;
#7534 = CARTESIAN_POINT ( 'NONE',  ( -1.477846259693498254, 49.81903562097207327, 59.21119304902337888 ) ) ;
#7535 = CARTESIAN_POINT ( 'NONE',  ( -3.350035803220276609, 49.20851703305431357, 92.13308880123798872 ) ) ;
#7536 = DIRECTION ( 'NONE',  ( 1.000000000000000000, -0.000000000000000000, -0.000000000000000000 ) ) ;
#7537 = LINE ( 'NONE', #5941, #20 ) ;
#7538 = ADVANCED_FACE ( 'NONE', ( #1277 ), #13194, .T. ) ;
#7539 = CARTESIAN_POINT ( 'NONE',  ( -5.058133621542618030, 44.89684013992257405, 94.24246380294498238 ) ) ;
#7540 = VECTOR ( 'NONE', #11765, 1000.000000000000000 ) ;
#7541 = CARTESIAN_POINT ( 'NONE',  ( 2.522153740306495529, 49.81903562097208749, 83.21119304902340730 ) ) ;
#7542 =( NAMED_UNIT ( * ) SI_UNIT ( $, .STERADIAN. ) SOLID_ANGLE_UNIT ( ) );
#7543 = VECTOR ( 'NONE', #16161, 1000.000000000000000 ) ;
#7544 = FACE_OUTER_BOUND ( 'NONE', #8188, .T. ) ;
#7545 = FACE_OUTER_BOUND ( 'NONE', #15884, .T. ) ;
#7546 = CARTESIAN_POINT ( 'NONE',  ( -4.452986336060421380, 50.68046193778529585, 78.55837781537462661 ) ) ;
#7547 = PRESENTATION_STYLE_ASSIGNMENT (( #949 ) ) ;
#7548 = EDGE_CURVE ( 'NONE', #7434, #2442, #17238, .T. ) ;
#7549 = CARTESIAN_POINT ( 'NONE',  ( -8.311994772346579907, 42.89802645589339392, 78.33204358585338412 ) ) ;
#7550 = CARTESIAN_POINT ( 'NONE',  ( 8.647112560730464637, 43.05498688647372774, 77.35098120998416960 ) ) ;
#7551 = EDGE_CURVE ( 'NONE', #15360, #8218, #7769, .T. ) ;
#7552 = EDGE_LOOP ( 'NONE', ( #6433, #11676, #5347, #2602 ) ) ;
#7553 = VECTOR ( 'NONE', #8797, 1000.000000000000227 ) ;
#7554 = PLANE ( 'NONE',  #18574 ) ;
#7555 = CARTESIAN_POINT ( 'NONE',  ( 6.573693162767834330, 44.00881163587200717, 72.45432679953087529 ) ) ;
#7556 = EDGE_CURVE ( 'NONE', #5762, #7917, #1181, .T. ) ;
#7557 = LINE ( 'NONE', #12142, #4491 ) ;
#7558 = VECTOR ( 'NONE', #3103, 1000.000000000000000 ) ;
#7560 = EDGE_CURVE ( 'NONE', #129, #15570, #14364, .T. ) ;
#7559 = DIRECTION ( 'NONE',  ( 3.893792155548169402E-16, 7.183611964723547524E-17, -1.000000000000000000 ) ) ;
#7561 =( BOUNDED_CURVE ( )  B_SPLINE_CURVE ( 3, ( #2349, #8848, #5539, #10356 ),
 .UNSPECIFIED., .F., .F. ) 
 B_SPLINE_CURVE_WITH_KNOTS ( ( 4, 4 ),
 ( 1.735985064777024300, 1.737340566640508621 ),
 .UNSPECIFIED. ) 
 CURVE ( )  GEOMETRIC_REPRESENTATION_ITEM ( )  RATIONAL_B_SPLINE_CURVE ( ( 1.000000000000000000, 0.9999998468845641142, 0.9999998468845641142, 1.000000000000000000 ) ) 
 REPRESENTATION_ITEM ( '' )  );
#7562 = CARTESIAN_POINT ( 'NONE',  ( 5.675263920727823042, 51.29620106613522523, 77.96371040190514634 ) ) ;
#7563 = CARTESIAN_POINT ( 'NONE',  ( -0.5863195729081845942, 39.16218137147968292, 93.30865272277779354 ) ) ;
#7564 = FACE_OUTER_BOUND ( 'NONE', #7675, .T. ) ;
#7565 = CARTESIAN_POINT ( 'NONE',  ( 4.394343283833276992, 39.11584570990505938, 92.60183880123797451 ) ) ;
#7566 = ADVANCED_FACE ( 'NONE', ( #14248 ), #6264, .F. ) ;
#7567 = CARTESIAN_POINT ( 'NONE',  ( -0.9186189192224099020, 52.84343824287718405, 78.59945191334355741 ) ) ;
#7568 = ORIENTED_EDGE ( 'NONE', *, *, #16650, .F. ) ;
#7569 = CARTESIAN_POINT ( 'NONE',  ( -0.9988176903691428077, 49.83852402762217082, 91.89871380123798872 ) ) ;
#7570 = AXIS2_PLACEMENT_3D ( 'NONE', #2507, #7283, #18350 ) ;
#7571 = CARTESIAN_POINT ( 'NONE',  ( 0.5221537403065114047, 44.16218137147969713, 45.55433879953100273 ) ) ;
#7573 = CARTESIAN_POINT ( 'NONE',  ( 5.753005855668248181, 51.23877623043087937, 78.93669174070734584 ) ) ;
#7572 = AXIS2_PLACEMENT_3D ( 'NONE', #16473, #3684, #282 ) ;
#7574 = CARTESIAN_POINT ( 'NONE',  ( 5.555396287804228450, 50.63010651601021550, 77.16780247135808679 ) ) ;
#7575 = ORIENTED_EDGE ( 'NONE', *, *, #6724, .F. ) ;
#7576 = DIRECTION ( 'NONE',  ( -1.540237394707284467E-16, -1.793354297423764243E-16, 1.000000000000000000 ) ) ;
#7577 = CARTESIAN_POINT ( 'NONE',  ( -3.981178359372548492, 46.76218137147973408, 92.91433880294496817 ) ) ;
#7578 = ORIENTED_EDGE ( 'NONE', *, *, #354, .F. ) ;
#7579 = CARTESIAN_POINT ( 'NONE',  ( 5.666884522201894647, 41.76315400873614436, 94.43871379782397923 ) ) ;
#7580 = DIRECTION ( 'NONE',  ( 1.540237394707284220E-16, 1.793354297423764243E-16, -1.000000000000000000 ) ) ;
#7581 = DIRECTION ( 'NONE',  ( 0.5813877811927011807, -0.8136266022444372803, -5.636455622144619183E-17 ) ) ;
#7582 = CARTESIAN_POINT ( 'NONE',  ( 35.92215374030650565, 36.96218137147968719, 93.55433879953098142 ) ) ;
#7583 = DIRECTION ( 'NONE',  ( -1.000000000000000000, -1.402518428993831676E-16, -1.196361017915039239E-16 ) ) ;
#7584 = ADVANCED_FACE ( 'NONE', ( #20628, #7666, #4351 ), #5859, .F. ) ;
#7585 = CARTESIAN_POINT ( 'NONE',  ( -3.131615841865540428, 36.83467417924890697, 78.81697279211699936 ) ) ;
#7586 = ORIENTED_EDGE ( 'NONE', *, *, #9125, .F. ) ;
#7587 = CARTESIAN_POINT ( 'NONE',  ( 2.522153740306510183, 50.16218137147969713, 58.55433879953100984 ) ) ;
#7588 = VECTOR ( 'NONE', #8756, 1000.000000000000000 ) ;
#7589 = CARTESIAN_POINT ( 'NONE',  ( -3.628867371436363953, 48.69222599884265179, 93.57933879782399345 ) ) ;
#7590 = VERTEX_POINT ( 'NONE', #14144 ) ;
#7591 = DIRECTION ( 'NONE',  ( -0.3165065846431826535, -0.9485903129789529098, -2.188653791613874008E-16 ) ) ;
#7592 = CARTESIAN_POINT ( 'NONE',  ( -4.524181921268124462, 40.28999182795290324, 93.53933880123797451 ) ) ;
#7593 = B_SPLINE_CURVE_WITH_KNOTS ( 'NONE', 3,
 ( #4671, #6804, #1505, #3405 ),
 .UNSPECIFIED., .F., .F.,
 ( 4, 4 ),
 ( 0.01304472255648652691, 0.01428392225856168346 ),
 .UNSPECIFIED. ) ;
#7594 = PLANE ( 'NONE',  #11014 ) ;
#7595 = CARTESIAN_POINT ( 'NONE',  ( 10.77494014480653561, 42.96218137147968008, 77.40433879953098995 ) ) ;
#7596 = CARTESIAN_POINT ( 'NONE',  ( 0.7901638384306272078, 50.30062182352762079, 94.82933879782397923 ) ) ;
#7597 = DIRECTION ( 'NONE',  ( -1.402518428993831676E-16, 1.000000000000000000, 0.000000000000000000 ) ) ;
#7598 = ORIENTED_EDGE ( 'NONE', *, *, #8884, .F. ) ;
#7599 = FACE_OUTER_BOUND ( 'NONE', #16701, .T. ) ;
#7600 = ORIENTED_EDGE ( 'NONE', *, *, #901, .T. ) ;
#7601 = VECTOR ( 'NONE', #15764, 1000.000000000000227 ) ;
#7602 = LINE ( 'NONE', #20465, #6790 ) ;
#7603 = CARTESIAN_POINT ( 'NONE',  ( 2.043125170982144745, 38.48583871533720213, 93.92996380123798872 ) ) ;
#7604 = CARTESIAN_POINT ( 'NONE',  ( 5.712782733624313103, 51.26848743039855094, 75.36064185147203887 ) ) ;
#7605 = ORIENTED_EDGE ( 'NONE', *, *, #10821, .T. ) ;
#7606 = CARTESIAN_POINT ( 'NONE',  ( 6.660594192354429843, 43.89417127335556046, 94.36058879782399345 ) ) ;
#7607 = CARTESIAN_POINT ( 'NONE',  ( 8.787829143201870252, 41.13140593384865440, 78.45948585835439815 ) ) ;
#7608 = ORIENTED_EDGE ( 'NONE', *, *, #10312, .F. ) ;
#7609 = CARTESIAN_POINT ( 'NONE',  ( 4.394267649348433835, 36.11327998621098345, 76.69403369658814995 ) ) ;
#7610 = CARTESIAN_POINT ( 'NONE',  ( 2.563360104887394630, 38.63792983641098289, 95.05433879953099563 ) ) ;
#7611 = ORIENTED_EDGE ( 'NONE', *, *, #17284, .T. ) ;
#7612 = CARTESIAN_POINT ( 'NONE',  ( -1.677846259693499542, 50.36218137147968577, 54.55433879953098852 ) ) ;
#7613 = CARTESIAN_POINT ( 'NONE',  ( 4.394343283833276992, 39.11584570990505938, 91.50808880123798872 ) ) ;
#7614 = ORIENTED_EDGE ( 'NONE', *, *, #3343, .F. ) ;
#7615 = B_SPLINE_CURVE_WITH_KNOTS ( 'NONE', 3,
 ( #18914, #10855, #20605, #16048, #2950, #1572, #17427, #3169, #12844, #11056, #9566, #11372, #1157, #9455 ),
 .UNSPECIFIED., .F., .F.,
 ( 4, 2, 2, 2, 2, 2, 4 ),
 ( 0.000000000000000000, 0.0005039684972345963082, 0.001007936994469192616, 0.001259921243086484103, 0.001511905491703775806, 0.001763889740321067509, 0.002015873988938359212 ),
 .UNSPECIFIED. ) ;
#7616 = CARTESIAN_POINT ( 'NONE',  ( 0.4527646634920744484, 35.36245494641288190, 80.45433879953087342 ) ) ;
#7617 = CARTESIAN_POINT ( 'NONE',  ( 4.393996117251955269, 36.11308595931626542, 76.96022115247204454 ) ) ;
#7618 = CARTESIAN_POINT ( 'NONE',  ( -1.876873622437038369, 39.01745058958429269, 91.62621379782397923 ) ) ;
#7619 = CIRCLE ( 'NONE', #130, 3.999999999999996447 ) ;
#7620 = CARTESIAN_POINT ( 'NONE',  ( 5.443310442819001338, 36.86288755851700927, 76.23948081211554495 ) ) ;
#7621 = CARTESIAN_POINT ( 'NONE',  ( 8.794665453373390562, 41.15189478912013499, 76.14505377247542128 ) ) ;
#7622 = EDGE_CURVE ( 'NONE', #10043, #16288, #11171, .T. ) ;
#7623 = LINE ( 'NONE', #14003, #9269 ) ;
#7624 = ORIENTED_EDGE ( 'NONE', *, *, #9893, .F. ) ;
#7625 = CARTESIAN_POINT ( 'NONE',  ( 2.115006173568111159, 52.20151759559819737, 76.48963291717792856 ) ) ;
#7626 = ORIENTED_EDGE ( 'NONE', *, *, #12708, .T. ) ;
#7627 = CARTESIAN_POINT ( 'NONE',  ( 6.740887235739653427, 50.50906804926147942, 75.70960632971019777 ) ) ;
#7628 = DIRECTION ( 'NONE',  ( -1.402518428993831183E-16, 1.000000000000000000, -3.469446951953617640E-16 ) ) ;
#7629 = CARTESIAN_POINT ( 'NONE',  ( -3.350035803220276609, 49.20851703305431357, 95.72683880123798872 ) ) ;
#7630 = CARTESIAN_POINT ( 'NONE',  ( -3.463632283681914892, 51.32894902012767346, 75.51931251450895388 ) ) ;
#7631 = ORIENTED_EDGE ( 'NONE', *, *, #21034, .F. ) ;
#7632 = ORIENTED_EDGE ( 'NONE', *, *, #10439, .T. ) ;
#7633 = CARTESIAN_POINT ( 'NONE',  ( -3.632453822589317038, 37.21544096238353205, 75.46341390175899733 ) ) ;
#7634 = CARTESIAN_POINT ( 'NONE',  ( -5.044287576081563529, 45.27497882680665242, 92.45433879953097289 ) ) ;
#7635 = ORIENTED_EDGE ( 'NONE', *, *, #12787, .T. ) ;
#7636 = LINE ( 'NONE', #15731, #12504 ) ;
#7637 = CARTESIAN_POINT ( 'NONE',  ( -6.803379318247109175, 40.47719848869107295, 79.07692288227858057 ) ) ;
#7638 = CARTESIAN_POINT ( 'NONE',  ( 7.776991732576825633, 40.48304684739793657, 75.69429397690826988 ) ) ;
#7639 = ORIENTED_EDGE ( 'NONE', *, *, #19619, .F. ) ;
#7640 = CARTESIAN_POINT ( 'NONE',  ( -4.799158982053665312, 37.15240611894267886, 77.91201545794896788 ) ) ;
#7641 = CARTESIAN_POINT ( 'NONE',  ( -7.157701799267968568, 41.72896584388870167, 79.54775079867083321 ) ) ;
#7642 = LINE ( 'NONE', #14123, #8837 ) ;
#7643 = CARTESIAN_POINT ( 'NONE',  ( 5.568489401881125289, 48.03437091500646261, 90.57058880123798872 ) ) ;
#7644 = CARTESIAN_POINT ( 'NONE',  ( -7.507604988220665909, 45.82440120099734315, 72.45433879953085921 ) ) ;
#7645 = CARTESIAN_POINT ( 'NONE',  ( 5.385255718775495026, 47.76702405936703855, 72.45432679953087529 ) ) ;
#7646 = ADVANCED_FACE ( 'NONE', ( #1385 ), #10877, .T. ) ;
#7647 = CARTESIAN_POINT ( 'NONE',  ( 1.256812508749381774, 49.74246873332880625, 92.67996380294498238 ) ) ;
#7648 = B_SPLINE_CURVE_WITH_KNOTS ( 'NONE', 3,
 ( #16978, #1988, #14965, #18256, #19844, #5264, #11781, #10192, #16675, #2094, #8595, #489 ),
 .UNSPECIFIED., .F., .F.,
 ( 4, 2, 2, 2, 2, 4 ),
 ( 8.673617379884034509E-19, 0.0001269736000813090034, 0.0001904604001219685602, 0.0002539472001626280899, 0.0003809208002439511066, 0.0005078944003252741776 ),
 .UNSPECIFIED. ) ;
#7649 = LINE ( 'NONE', #1163, #4815 ) ;
#7650 = CARTESIAN_POINT ( 'NONE',  ( 8.365446634792766289, 41.78557434852172747, 78.83412695248559032 ) ) ;
#7651 = CARTESIAN_POINT ( 'NONE',  ( 4.722153740306502812, 44.16218137147969003, 45.55433879953098852 ) ) ;
#7652 = CARTESIAN_POINT ( 'NONE',  ( -10.17784625969349754, 51.36218137147968577, 80.55433879953099563 ) ) ;
#7653 = CARTESIAN_POINT ( 'NONE',  ( 5.184346195580738836, 46.85389944054460898, 93.43362681315548457 ) ) ;
#7654 = CARTESIAN_POINT ( 'NONE',  ( 8.685073573159321825, 40.82344097173932340, 79.49103220525971381 ) ) ;
#7655 = CARTESIAN_POINT ( 'NONE',  ( 6.828503391016846891, 43.33193468930419101, 91.66433880123796030 ) ) ;
#7656 = CARTESIAN_POINT ( 'NONE',  ( -7.551054721414131699, 42.94398425051771540, 79.08626245367327101 ) ) ;
#7657 = CARTESIAN_POINT ( 'NONE',  ( 0.5221537403065188432, 44.16218137147969003, 54.55433879953099563 ) ) ;
#7658 = EDGE_CURVE ( 'NONE', #14841, #9248, #12360, .T. ) ;
#7659 = EDGE_LOOP ( 'NONE', ( #11228, #19643, #13170, #7008 ) ) ;
#7660 = CARTESIAN_POINT ( 'NONE',  ( 8.221673622452696506, 41.34128174147134871, 78.82488780898647462 ) ) ;
#7661 = CARTESIAN_POINT ( 'NONE',  ( -7.617292153972126556, 43.16748516956134551, 72.45433879953085921 ) ) ;
#7662 = DIRECTION ( 'NONE',  ( -0.5813877811927011807, 0.8136266022444372803, 5.636455622144619183E-17 ) ) ;
#7663 = FACE_OUTER_BOUND ( 'NONE', #20251, .T. ) ;
#7664 = CARTESIAN_POINT ( 'NONE',  ( 31.07218010054375412, 42.96218137147968008, 69.40574467885102194 ) ) ;
#7665 = CARTESIAN_POINT ( 'NONE',  ( -3.467962453771611830, 40.50591351489411096, 93.18871379611699979 ) ) ;
#7666 = FACE_OUTER_BOUND ( 'NONE', #11935, .T. ) ;
#7667 = EDGE_CURVE ( 'NONE', #867, #12950, #10983, .T. ) ;
#7668 = ADVANCED_FACE ( 'NONE', ( #6058 ), #6165, .T. ) ;
#7669 = ADVANCED_FACE ( 'NONE', ( #20838 ), #14048, .F. ) ;
#7670 = EDGE_LOOP ( 'NONE', ( #9084, #2388 ) ) ;
#7671 = CARTESIAN_POINT ( 'NONE',  ( 4.394343283833276992, 39.11584570990505938, 92.60183880123797451 ) ) ;
#7672 = CARTESIAN_POINT ( 'NONE',  ( 0.6746983353010208573, 52.36079151674319831, 78.91894492505406333 ) ) ;
#7673 = EDGE_CURVE ( 'NONE', #8340, #11453, #11084, .T. ) ;
#7674 = CARTESIAN_POINT ( 'NONE',  ( 5.770850603891227060, 51.22559503374887413, 77.28904345712264501 ) ) ;
#7675 = EDGE_LOOP ( 'NONE', ( #19789, #12530, #18162, #8122 ) ) ;
#7676 = LINE ( 'NONE', #2984, #20721 ) ;
#7677 = CARTESIAN_POINT ( 'NONE',  ( -3.981178359372548492, 46.76218137147973408, 94.16433880294496817 ) ) ;
#7678 = SHAPE_REPRESENTATION ( 'Locking Springs', ( #18366 ), #9896 ) ;
#7679 = ORIENTED_EDGE ( 'NONE', *, *, #14442, .T. ) ;
#7680 = DIRECTION ( 'NONE',  ( 1.402518428993831676E-16, -1.000000000000000000, 0.000000000000000000 ) ) ;
#7681 = CARTESIAN_POINT ( 'NONE',  ( -0.9315166138311854471, 52.97860336813545246, 76.61976384666378692 ) ) ;
#7682 = CARTESIAN_POINT ( 'NONE',  ( -4.402123124950023225, 50.71898518566671044, 76.03313496065364063 ) ) ;
#7683 = DIRECTION ( 'NONE',  ( -0.3165065846431827090, -0.9485903129789527988, 0.000000000000000000 ) ) ;
#7684 = FACE_OUTER_BOUND ( 'NONE', #17994, .T. ) ;
#7685 = CARTESIAN_POINT ( 'NONE',  ( -3.299506883664278245, 36.95868852876193955, 79.18890841331918296 ) ) ;
#7686 = ORIENTED_EDGE ( 'NONE', *, *, #8034, .T. ) ;
#7687 = CARTESIAN_POINT ( 'NONE',  ( 6.813511439209503529, 39.88797755036236481, 72.45433879953087342 ) ) ;
#7688 = CARTESIAN_POINT ( 'NONE',  ( -4.007890887056451135, 40.01116025973682611, 92.64183879782400766 ) ) ;
#7689 = ORIENTED_EDGE ( 'NONE', *, *, #2211, .F. ) ;
#7690 = CARTESIAN_POINT ( 'NONE',  ( -4.567115856812060670, 47.10047254335474065, 94.55496380123798872 ) ) ;
#7691 = CARTESIAN_POINT ( 'NONE',  ( 6.198496396448986090, 45.68315280215533392, 95.33621380123798872 ) ) ;
#7692 = CARTESIAN_POINT ( 'NONE',  ( 30.92220646078100188, 42.96218137147968008, 61.80715055817104542 ) ) ;
#7693 = CARTESIAN_POINT ( 'NONE',  ( -4.225674986753855222, 37.47641307392585475, 77.99882451231113123 ) ) ;
#7694 = EDGE_CURVE ( 'NONE', #1468, #3866, #7983, .T. ) ;
#7695 = PLANE ( 'NONE',  #8930 ) ;
#7696 = ORIENTED_EDGE ( 'NONE', *, *, #4693, .F. ) ;
#7697 = ADVANCED_FACE ( 'NONE', ( #7564 ), #1815, .T. ) ;
#7698 = CARTESIAN_POINT ( 'NONE',  ( 8.267857704931044438, 41.47037322861213937, 75.97962990480824885 ) ) ;
#7699 = EDGE_CURVE ( 'NONE', #8464, #57, #3501, .T. ) ;
#7700 = EDGE_LOOP ( 'NONE', ( #11150, #4063, #10581, #18113 ) ) ;
#7701 = VECTOR ( 'NONE', #1882, 1000.000000000000000 ) ;
#7702 = CARTESIAN_POINT ( 'NONE',  ( -3.188252658875160961, 51.40685744052633055, 75.70044805065693083 ) ) ;
#7703 = CARTESIAN_POINT ( 'NONE',  ( 4.394343283833276992, 39.11584570990505938, 94.00808880123797451 ) ) ;
#7704 = CARTESIAN_POINT ( 'NONE',  ( -7.121523164365337166, 41.57863559946763132, 78.20300316143082853 ) ) ;
#7705 = ORIENTED_EDGE ( 'NONE', *, *, #7762, .T. ) ;
#7706 = CARTESIAN_POINT ( 'NONE',  ( 0.2541436421823697334, 38.02374091943176637, 95.29808879782397923 ) ) ;
#7707 = CARTESIAN_POINT ( 'NONE',  ( 1.630627053521187086, 49.16218137147969003, 93.93365272277780775 ) ) ;
#7708 = ORIENTED_EDGE ( 'NONE', *, *, #5714, .T. ) ;
#7709 = CARTESIAN_POINT ( 'NONE',  ( 6.303853310235981056, 37.47779998508790555, 78.34126521887253602 ) ) ;
#7710 = CARTESIAN_POINT ( 'NONE',  ( 5.561690527597086486, 51.38009315662554854, 76.32883089164610624 ) ) ;
#7711 = ORIENTED_EDGE ( 'NONE', *, *, #10714, .F. ) ;
#7712 = PLANE ( 'NONE',  #335 ) ;
#7713 = CARTESIAN_POINT ( 'NONE',  ( 0.8124031970253874357, 52.35243704943727039, 78.79200666326234170 ) ) ;
#7714 = EDGE_LOOP ( 'NONE', ( #6545, #2224, #14240, #696, #13479 ) ) ;
#7715 = CARTESIAN_POINT ( 'NONE',  ( -5.404516697003497683, 49.82915726805031653, 78.31219776780484665 ) ) ;
#7716 = CARTESIAN_POINT ( 'NONE',  ( 6.006122683886344404, 43.48762228702367594, 95.05433879953098142 ) ) ;
#7717 = CARTESIAN_POINT ( 'NONE',  ( 4.673174852049362116, 39.63213674411673537, 93.11058879782397923 ) ) ;
#7718 = AXIS2_PLACEMENT_3D ( 'NONE', #1096, #14068, #5974 ) ;
#7719 = ITEM_DEFINED_TRANSFORMATION ( 'NONE', 'NONE', #16337,  #18366 ) ;
#7720 = CARTESIAN_POINT ( 'NONE',  ( 5.478721299898049679, 36.88819086051147167, 76.06572720930677178 ) ) ;
#7721 = CARTESIAN_POINT ( 'NONE',  ( 8.868817592801743643, 41.37413345511091478, 75.97198585835440099 ) ) ;
#7722 = CARTESIAN_POINT ( 'NONE',  ( -3.494425977668756289, 37.11348535344146171, 77.68304435440727218 ) ) ;
#7723 = ORIENTED_EDGE ( 'NONE', *, *, #206, .T. ) ;
#7724 = EDGE_CURVE ( 'NONE', #10690, #19575, #1864, .T. ) ;
#7725 = CARTESIAN_POINT ( 'NONE',  ( 2.115006181195345558, 52.20151856286257441, 78.16610350541323271 ) ) ;
#7726 = VERTEX_POINT ( 'NONE', #14573 ) ;
#7727 = CARTESIAN_POINT ( 'NONE',  ( 11.22215374030650281, 39.96218137147969429, 54.55433879953099563 ) ) ;
#7728 = DIRECTION ( 'NONE',  ( 0.000000000000000000, -2.891205793294680792E-16, -1.000000000000000000 ) ) ;
#7729 = CARTESIAN_POINT ( 'NONE',  ( 3.460444912181559474, 49.25145096859824889, 93.14871380123798872 ) ) ;
#7730 = CARTESIAN_POINT ( 'NONE',  ( 8.872773925109784798, 41.38599083402314704, 79.54845644658969661 ) ) ;
#7731 = VERTEX_POINT ( 'NONE', #17766 ) ;
#7732 = ORIENTED_EDGE ( 'NONE', *, *, #12768, .T. ) ;
#7733 = VECTOR ( 'NONE', #5414, 1000.000000000000000 ) ;
#7734 = CARTESIAN_POINT ( 'NONE',  ( -3.970777706820451058, 37.46534718714770662, 75.37821288891845484 ) ) ;
#7735 = LINE ( 'NONE', #4627, #4391 ) ;
#7736 = CARTESIAN_POINT ( 'NONE',  ( -6.727933487834448556, 40.33118276386390022, 78.21032190485932745 ) ) ;
#7737 = ORIENTED_EDGE ( 'NONE', *, *, #11523, .F. ) ;
#7738 = CARTESIAN_POINT ( 'NONE',  ( 4.591414450663933167, 52.09679700955160797, 78.70655549710109256 ) ) ;
#7739 = CARTESIAN_POINT ( 'NONE',  ( 8.215380408549069813, 41.33579643961174810, 77.32915800260404637 ) ) ;
#7740 = CARTESIAN_POINT ( 'NONE',  ( 8.386307069575464013, 39.92801880710491957, 76.83374382764255017 ) ) ;
#7741 = VERTEX_POINT ( 'NONE', #9794 ) ;
#7742 = CARTESIAN_POINT ( 'NONE',  ( 6.522560395309022319, 49.75102024682771429, 76.63889762306028786 ) ) ;
#7743 = LINE ( 'NONE', #19432, #5325 ) ;
#7744 = CARTESIAN_POINT ( 'NONE',  ( 6.434733849016518903, 38.48046520452516717, 76.20198684891533958 ) ) ;
#7745 = CARTESIAN_POINT ( 'NONE',  ( -4.524181921268124462, 40.28999182795290324, 93.69558880123800293 ) ) ;
#7746 = AXIS2_PLACEMENT_3D ( 'NONE', #14671, #17763, #8077 ) ;
#7747 = SHAPE_REPRESENTATION_RELATIONSHIP ( 'NONE' , 'NONE' ,  #9056, #19981 ) ;
#7748 = EDGE_CURVE ( 'NONE', #2200, #2739, #10689, .T. ) ;
#7749 = CARTESIAN_POINT ( 'NONE',  ( 6.408921161899227670, 38.45374572596151097, 77.78408325655041722 ) ) ;
#7750 = VECTOR ( 'NONE', #5052, 1000.000000000000000 ) ;
#7751 = CARTESIAN_POINT ( 'NONE',  ( 31.22215374030650281, 42.96218137147968008, 73.80433879953100984 ) ) ;
#7752 = CARTESIAN_POINT ( 'NONE',  ( 5.197291232937072181, 37.60686682075191811, 75.36061873398452349 ) ) ;
#7753 = CARTESIAN_POINT ( 'NONE',  ( -0.9377747940352504363, 52.97987797655117959, 77.77566232894263010 ) ) ;
#7754 = CARTESIAN_POINT ( 'NONE',  ( -12.18117835937254867, 39.56218137147966019, 95.05433879953098142 ) ) ;
#7755 = CARTESIAN_POINT ( 'NONE',  ( 25.63948732994507651, 36.35905713404684292, 74.70433879953100131 ) ) ;
#7756 = CARTESIAN_POINT ( 'NONE',  ( 5.600448134661695221, 51.35146447353857013, 76.04240903267428564 ) ) ;
#7757 = VECTOR ( 'NONE', #19247, 1000.000000000000000 ) ;
#7758 = EDGE_LOOP ( 'NONE', ( #14190, #8199, #15402, #18015, #5203 ) ) ;
#7759 = CARTESIAN_POINT ( 'NONE',  ( -7.650389079877051302, 47.48727607949400209, 78.95058778273427436 ) ) ;
#7760 = CARTESIAN_POINT ( 'NONE',  ( 5.670718203856349504, 37.02538481862475805, 75.97247164366282846 ) ) ;
#7761 = EDGE_LOOP ( 'NONE', ( #5310, #20906, #2355, #1971, #13233, #18325 ) ) ;
#7762 = EDGE_CURVE ( 'NONE', #7140, #1086, #8089, .T. ) ;
#7763 = DIRECTION ( 'NONE',  ( 0.3181025035073955509, -0.9480563259966822143, -1.210247515173838859E-16 ) ) ;
#7764 = CARTESIAN_POINT ( 'NONE',  ( -4.051275123961953106, 50.96833819619023842, 76.11298501741460143 ) ) ;
#7765 = CARTESIAN_POINT ( 'NONE',  ( -4.796313072339923878, 37.15030396007738744, 78.92026643871187730 ) ) ;
#7766 = CARTESIAN_POINT ( 'NONE',  ( -4.283496025856504019, 47.84326572019833179, 72.45432679953087529 ) ) ;
#7767 = LINE ( 'NONE', #19051, #15215 ) ;
#7768 = CARTESIAN_POINT ( 'NONE',  ( 9.348820989215322896, 42.81273408501008504, 77.37738884012668450 ) ) ;
#7769 = LINE ( 'NONE', #4660, #13518 ) ;
#7770 = APPLICATION_CONTEXT ( 'automotive_design' ) ;
#7771 = AXIS2_PLACEMENT_3D ( 'NONE', #7253, #20118, #18537 ) ;
#7772 = EDGE_CURVE ( 'NONE', #11143, #16863, #300, .T. ) ;
#7773 = CARTESIAN_POINT ( 'NONE',  ( 8.789256573544017570, 41.13568403313856692, 78.71078388337100762 ) ) ;
#7774 = PLANE ( 'NONE',  #14998 ) ;
#7775 = CARTESIAN_POINT ( 'NONE',  ( -3.058525104374893111, 36.78526957849948786, 76.85386088035156149 ) ) ;
#7776 = EDGE_LOOP ( 'NONE', ( #1632, #13286, #7085, #12104, #7165, #10205 ) ) ;
#7777 = DIRECTION ( 'NONE',  ( -1.402518428993831183E-16, 1.000000000000000000, -3.469446951953617640E-16 ) ) ;
#7778 = CARTESIAN_POINT ( 'NONE',  ( -0.2125050281363792815, 38.58189400963055959, 90.80496380294498238 ) ) ;
#7779 = ORIENTED_EDGE ( 'NONE', *, *, #4930, .T. ) ;
#7780 = CARTESIAN_POINT ( 'NONE',  ( 5.431796663225051169, 50.72292504519191425, 78.93490712750880789 ) ) ;
#7781 = CIRCLE ( 'NONE', #12882, 6.200000000000000178 ) ;
#7782 = DIRECTION ( 'NONE',  ( -1.540237394707284220E-16, -1.793354297423764243E-16, 1.000000000000000000 ) ) ;
#7783 = CARTESIAN_POINT ( 'NONE',  ( 8.217283821720865689, 41.37630060163266421, 77.88643322029270166 ) ) ;
#7784 = DIRECTION ( 'NONE',  ( -1.084202172485505420E-16, -1.000000000000000000, 0.000000000000000000 ) ) ;
#7785 = CARTESIAN_POINT ( 'NONE',  ( 0.8361026161131213108, 52.35223742288051341, 76.13704228601427815 ) ) ;
#7786 = CARTESIAN_POINT ( 'NONE',  ( 8.378637954445377289, 41.81363803720061867, 78.41904468188381827 ) ) ;
#7787 = VERTEX_POINT ( 'NONE', #20932 ) ;
#7788 = CARTESIAN_POINT ( 'NONE',  ( 5.731194756759665054, 37.06859914914154075, 77.74321050730907245 ) ) ;
#7789 = ORIENTED_EDGE ( 'NONE', *, *, #16125, .T. ) ;
#7790 = CARTESIAN_POINT ( 'NONE',  ( 6.198496396448986090, 45.68315280215533392, 94.08621380123798872 ) ) ;
#7791 = CARTESIAN_POINT ( 'NONE',  ( -7.306900047088299210, 46.60106584047063194, 79.40728616877404988 ) ) ;
#7792 = CARTESIAN_POINT ( 'NONE',  ( 6.813511439209503529, 39.88797755036236481, 75.45433879953087342 ) ) ;
#7793 = CARTESIAN_POINT ( 'NONE',  ( 5.729336661111230633, 37.06727142202039715, 75.98270377909689444 ) ) ;
#7794 = FACE_OUTER_BOUND ( 'NONE', #20443, .T. ) ;
#7795 = AXIS2_PLACEMENT_3D ( 'NONE', #12853, #1584, #11275 ) ;
#7796 = EDGE_LOOP ( 'NONE', ( #19856, #15897, #9925, #15276 ) ) ;
#7797 = CARTESIAN_POINT ( 'NONE',  ( 4.640492351041169528, 52.06054514152135937, 78.02172882224894579 ) ) ;
#7798 =( BOUNDED_CURVE ( )  B_SPLINE_CURVE ( 2, ( #10261, #16736, #2575, #20744, #20641, #4168, #10997, #4263, #1293, #14157, #12575 ),
 .UNSPECIFIED., .F., .F. ) 
 B_SPLINE_CURVE_WITH_KNOTS ( ( 3, 2, 2, 2, 2, 3 ),
 ( 0.3333811345117426717, 0.3499999999999999778, 0.3750000000000000000, 0.4000000000000000222, 0.4249999999999999889, 0.4333811345117426495 ),
 .UNSPECIFIED. ) 
 CURVE ( )  GEOMETRIC_REPRESENTATION_ITEM ( )  RATIONAL_B_SPLINE_CURVE ( ( 0.9660722070828662300, 0.9493985675960723292, 1.000000000000000000, 0.9238795325112867385, 1.000000000000000000, 0.9238795325112867385, 1.000000000000000000, 0.9238795325112867385, 1.000000000000000000, 0.9744809649152144093, 0.9660722070828662300 ) ) 
 REPRESENTATION_ITEM ( '' )  );
#7799 = ORIENTED_EDGE ( 'NONE', *, *, #20025, .T. ) ;
#7800 = AXIS2_PLACEMENT_3D ( 'NONE', #5708, #4007, #20500 ) ;
#7801 = CARTESIAN_POINT ( 'NONE',  ( -2.929408986750495103, 51.59181765175492274, 76.33204918460485544 ) ) ;
#7802 = AXIS2_PLACEMENT_3D ( 'NONE', #2120, #6987, #3809 ) ;
#7803 = CARTESIAN_POINT ( 'NONE',  ( -2.904223097202481174, 48.62752260303690122, 91.27371379953098085 ) ) ;
#7804 = CARTESIAN_POINT ( 'NONE',  ( -7.136096162509048213, 41.62471999620901641, 78.11653805097020609 ) ) ;
#7805 = ORIENTED_EDGE ( 'NONE', *, *, #7551, .T. ) ;
#7806 = EDGE_CURVE ( 'NONE', #4618, #14094, #19458, .T. ) ;
#7807 = CARTESIAN_POINT ( 'NONE',  ( -5.367147075874662221, 49.84972784727108319, 78.71528818263502103 ) ) ;
#7808 = CARTESIAN_POINT ( 'NONE',  ( -4.845820878285513444, 46.15288543214547445, 95.05433879953095300 ) ) ;
#7809 = ORIENTED_EDGE ( 'NONE', *, *, #5694, .T. ) ;
#7810 = CARTESIAN_POINT ( 'NONE',  ( 5.333553402713407721, 50.79397291885030086, 75.97344461144770378 ) ) ;
#7811 = ADVANCED_FACE ( 'NONE', ( #6368 ), #13085, .F. ) ;
#7812 = ORIENTED_EDGE ( 'NONE', *, *, #19670, .T. ) ;
#7813 = CIRCLE ( 'NONE', #14614, 0.5999999999999928724 ) ;
#7814 = DIRECTION ( 'NONE',  ( 1.540237394707284220E-16, 1.793354297423764243E-16, -1.000000000000000000 ) ) ;
#7815 = VECTOR ( 'NONE', #16135, 1000.000000000000000 ) ;
#7816 = CARTESIAN_POINT ( 'NONE',  ( -5.784195910403845176, 44.99242805365518194, 91.03933880123798872 ) ) ;
#7817 = B_SPLINE_CURVE_WITH_KNOTS ( 'NONE', 3,
 ( #7502, #4395, #9215, #14402, #7709, #15905, #20474, #11120, #20871, #1324, #14188, #11022, #5908, #20771, #4292, #19185, #17390, #20574, #2709 ),
 .UNSPECIFIED., .F., .F.,
 ( 4, 1, 1, 1, 1, 1, 1, 1, 1, 1, 1, 1, 1, 1, 1, 1, 4 ),
 ( 0.000000000000000000, 0.07116601901339190961, 0.1384582187113551910, 0.2014355002094309066, 0.2607329607935783833, 0.3172301401005571675, 0.3704881719161017273, 0.4221645193212664182, 0.4717967126376631515, 0.5218096718684601676, 0.5745631757277218643, 0.6310618342314253670, 0.6925022631777019155, 0.7595319055140381526, 0.8328598856178031085, 0.9128843800434378597, 0.9999999999999998890 ),
 .UNSPECIFIED. ) ;
#7818 = VERTEX_POINT ( 'NONE', #11396 ) ;
#7819 = CARTESIAN_POINT ( 'NONE',  ( 4.722153740306502812, 44.16218137147969003, 54.55433879953099563 ) ) ;
#7820 = CARTESIAN_POINT ( 'NONE',  ( 5.775515014206123787, 42.15321788283623761, 95.05433879953102405 ) ) ;
#7821 = ADVANCED_FACE ( 'NONE', ( #16387 ), #6290, .F. ) ;
#7822 = CARTESIAN_POINT ( 'NONE',  ( 0.8481543884537371403, 52.95614222172972063, 78.61836828546933020 ) ) ;
#7823 = CARTESIAN_POINT ( 'NONE',  ( 5.856396280011940902, 46.10368687828906076, 92.09496379782399345 ) ) ;
#7824 = AXIS2_PLACEMENT_3D ( 'NONE', #16353, #19632, #16558 ) ;
#7825 = CARTESIAN_POINT ( 'NONE',  ( -3.682072889308528385, 36.32725962120449736, 77.89282216559597316 ) ) ;
#7826 = EDGE_CURVE ( 'NONE', #13483, #11825, #9556, .T. ) ;
#7827 = DIRECTION ( 'NONE',  ( -0.3165065846431826535, -0.9485903129789527988, 0.000000000000000000 ) ) ;
#7828 = CARTESIAN_POINT ( 'NONE',  ( -3.537323694296536036, 36.22033922170236053, 77.24173421363296654 ) ) ;
#7829 = ORIENTED_EDGE ( 'NONE', *, *, #20523, .F. ) ;
#7830 = CARTESIAN_POINT ( 'NONE',  ( 1.232152210925365976, 52.93468634029516551, 76.77372409715140122 ) ) ;
#7831 = VECTOR ( 'NONE', #13733, 1000.000000000000000 ) ;
#7832 = CARTESIAN_POINT ( 'NONE',  ( -3.362469148716389800, 37.00519621768119549, 77.78682928037112276 ) ) ;
#7833 = VERTEX_POINT ( 'NONE', #20595 ) ;
#7834 = CARTESIAN_POINT ( 'NONE',  ( -7.776276679187434482, 41.23368414744241761, 78.54947220199125013 ) ) ;
#7835 = CARTESIAN_POINT ( 'NONE',  ( 5.731194756759665054, 37.06859914914154075, 77.74321050730907245 ) ) ;
#7836 = CARTESIAN_POINT ( 'NONE',  ( 11.22215374030650281, 42.96218137147968008, 69.80574467885101342 ) ) ;
#7837 = B_SPLINE_SURFACE_WITH_KNOTS ( 'NONE', 3, 1, ( 
 ( #17978, #3402 ),
 ( #8632, #19879 ),
 ( #10229, #6801 ),
 ( #7000, #18088 ),
 ( #16707, #19671 ),
 ( #14885, #4986 ),
 ( #15112, #14681 ),
 ( #518, #307 ),
 ( #5197, #9913 ),
 ( #13306, #3512 ),
 ( #5403, #13501 ),
 ( #13197, #11616 ),
 ( #8193, #15002 ),
 ( #2130, #11924 ),
 ( #16495, #108 ) ),
 .UNSPECIFIED., .F., .F., .F.,
 ( 4, 1, 1, 1, 1, 1, 1, 1, 1, 1, 1, 1, 4 ),
 ( 2, 2 ),
 ( 0.000000000000000000, 0.1159675137638946224, 0.2163545172648820292, 0.3041323377849299292, 0.3879046361115746633, 0.4329802283776429395, 0.4868190193916722697, 0.5485431915433492955, 0.6192726642024330985, 0.7001311270025748490, 0.7903233920492748199, 0.8897556754282296421, 1.000000000000000000 ),
 ( 0.000000000000000000, 1.000000000000000000 ),
 .UNSPECIFIED. ) ;
#7838 = CARTESIAN_POINT ( 'NONE',  ( 8.807144941123576487, 41.18929660559136607, 79.54516904849367620 ) ) ;
#7839 = ORIENTED_EDGE ( 'NONE', *, *, #3886, .T. ) ;
#7840 = FACE_OUTER_BOUND ( 'NONE', #19090, .T. ) ;
#7841 = ORIENTED_EDGE ( 'NONE', *, *, #19447, .F. ) ;
#7842 = VECTOR ( 'NONE', #18457, 1000.000000000000227 ) ;
#7843 = CARTESIAN_POINT ( 'NONE',  ( -3.791754179604009067, 37.33310971910048437, 75.41196988111011024 ) ) ;
#7844 = CARTESIAN_POINT ( 'NONE',  ( -4.579686653871015700, 36.99029075099881680, 76.02016401025396419 ) ) ;
#7845 = CARTESIAN_POINT ( 'NONE',  ( -5.404861408967762237, 49.82879706497137562, 76.56315823047148683 ) ) ;
#7846 = ORIENTED_EDGE ( 'NONE', *, *, #14708, .T. ) ;
#7847 = CARTESIAN_POINT ( 'NONE',  ( 26.43948732994507367, 36.35905713404684292, 74.70433879953098710 ) ) ;
#7848 = CARTESIAN_POINT ( 'NONE',  ( -5.160557796316017409, 37.41935686500600156, 77.90139762306027649 ) ) ;
#7849 = CARTESIAN_POINT ( 'NONE',  ( 3.052271114939394625, 39.76217992266624890, 95.01850673350041632 ) ) ;
#7850 = ORIENTED_EDGE ( 'NONE', *, *, #7405, .T. ) ;
#7851 = CARTESIAN_POINT ( 'NONE',  ( 5.496601215626250259, 37.64336993767980744, 77.46538603227857323 ) ) ;
#7852 = CARTESIAN_POINT ( 'NONE',  ( -7.606224546186219015, 40.66142810410499919, 79.38495514127318131 ) ) ;
#7853 = CARTESIAN_POINT ( 'NONE',  ( -4.677846259693495767, 44.16218127507053737, 93.01911326394946400 ) ) ;
#7854 = EDGE_CURVE ( 'NONE', #7247, #4065, #15321, .T. ) ;
#7855 = CARTESIAN_POINT ( 'NONE',  ( 4.454354847297358866, 39.79502961122975790, 90.27410626197791998 ) ) ;
#7856 = CARTESIAN_POINT ( 'NONE',  ( 5.345530521434427307, 50.61492889873513690, 75.36061482756318242 ) ) ;
#7857 = CARTESIAN_POINT ( 'NONE',  ( -7.885657102084565828, 41.56435211639550431, 79.54845644658969661 ) ) ;
#7858 = DIRECTION ( 'NONE',  ( -0.3165065846431827645, -0.9485903129789529098, 0.000000000000000000 ) ) ;
#7859 = CARTESIAN_POINT ( 'NONE',  ( -0.5518162899754186501, 52.21439382095001491, 79.25925238658010130 ) ) ;
#7860 = VERTEX_POINT ( 'NONE', #9660 ) ;
#7861 = CARTESIAN_POINT ( 'NONE',  ( -4.337980680445880921, 37.55764029813086324, 75.97325816659191844 ) ) ;
#7862 = LINE ( 'NONE', #1262, #5499 ) ;
#7863 = PLANE ( 'NONE',  #8904 ) ;
#7864 = CARTESIAN_POINT ( 'NONE',  ( -0.7268458593731681461, 40.36218137147969998, 45.55433879953100273 ) ) ;
#7865 = VECTOR ( 'NONE', #5319, 1000.000000000000114 ) ;
#7866 = ORIENTED_EDGE ( 'NONE', *, *, #10660, .T. ) ;
#7867 = ORIENTED_EDGE ( 'NONE', *, *, #1029, .F. ) ;
#7868 = CARTESIAN_POINT ( 'NONE',  ( -4.536533255567898770, 37.70852454801545406, 78.62737644262512049 ) ) ;
#7869 = CARTESIAN_POINT ( 'NONE',  ( -4.039512053894965149, 50.97623261712813303, 76.19470787560661051 ) ) ;
#7870 = CARTESIAN_POINT ( 'NONE',  ( 6.575642869179847416, 50.63112740639009246, 77.70577767651062118 ) ) ;
#7871 = CARTESIAN_POINT ( 'NONE',  ( -1.183761187420877548, 49.81017696809242068, 83.28180655319408743 ) ) ;
#7872 = CARTESIAN_POINT ( 'NONE',  ( -5.486992102393413617, 39.49954625374182626, 72.45432679953087529 ) ) ;
#7873 = CIRCLE ( 'NONE', #13995, 8.199999999999995737 ) ;
#7874 = CARTESIAN_POINT ( 'NONE',  ( 8.638939746224972183, 43.04959301625464008, 77.37738884012668450 ) ) ;
#7875 = DIRECTION ( 'NONE',  ( 0.9429220365244121993, -0.3330135628418984250, 8.551124769255302663E-17 ) ) ;
#7876 = CARTESIAN_POINT ( 'NONE',  ( 6.955656837306707807, 50.35042639603116044, 76.39262467917644983 ) ) ;
#7877 = STYLED_ITEM ( 'NONE', ( #7547 ), #18516 ) ;
#7878 = LINE ( 'NONE', #11399, #7507 ) ;
#7879 = EDGE_CURVE ( 'NONE', #8809, #10514, #6131, .T. ) ;
#7880 = DIRECTION ( 'NONE',  ( 1.000000000000000000, -0.000000000000000000, -0.000000000000000000 ) ) ;
#7881 = CARTESIAN_POINT ( 'NONE',  ( 0.5221537403065097394, 44.16218137147969003, 80.55433879953099563 ) ) ;
#7882 = ORIENTED_EDGE ( 'NONE', *, *, #15601, .T. ) ;
#7883 = VECTOR ( 'NONE', #8108, 1000.000000000000000 ) ;
#7884 = DIRECTION ( 'NONE',  ( -1.540237394707284467E-16, -1.793354297423764243E-16, 1.000000000000000000 ) ) ;
#7885 = AXIS2_PLACEMENT_3D ( 'NONE', #9948, #9525, #6407 ) ;
#7886 = CARTESIAN_POINT ( 'NONE',  ( 5.025485839985549319, 41.56218137147963887, 92.28933880294496817 ) ) ;
#7887 = ORIENTED_EDGE ( 'NONE', *, *, #1751, .F. ) ;
#7888 = CARTESIAN_POINT ( 'NONE',  ( -0.6485145178734266214, 52.21717837221741121, 75.74123345422913189 ) ) ;
#7889 = CARTESIAN_POINT ( 'NONE',  ( 8.793292705229012185, 41.14778057584590698, 77.83369646723784285 ) ) ;
#7890 = CARTESIAN_POINT ( 'NONE',  ( 6.012275498921958672, 37.26944915646792822, 78.37198585835440667 ) ) ;
#7891 = CARTESIAN_POINT ( 'NONE',  ( 31.07218010054375412, 45.56218137147968861, 64.80574467885102763 ) ) ;
#7892 = CARTESIAN_POINT ( 'NONE',  ( -0.9504375969237850441, 51.37401713635502887, 77.77566232894263010 ) ) ;
#7893 = VERTEX_POINT ( 'NONE', #19117 ) ;
#7894 = CARTESIAN_POINT ( 'NONE',  ( 2.522153740306504854, 47.62628298661744708, 85.15433879953098995 ) ) ;
#7895 = ORIENTED_EDGE ( 'NONE', *, *, #12906, .F. ) ;
#7896 = CARTESIAN_POINT ( 'NONE',  ( -7.723582874747322968, 47.23591325229828186, 72.45433879953087342 ) ) ;
#7897 = DIRECTION ( 'NONE',  ( 0.9999689119394085113, -0.007885122365275719011, 1.526048693634352652E-16 ) ) ;
#7898 = CARTESIAN_POINT ( 'NONE',  ( 0.3284977539024462323, 52.35989436107013972, 76.34474084658923232 ) ) ;
#7899 = VECTOR ( 'NONE', #3477, 1000.000000000000000 ) ;
#7900 = CARTESIAN_POINT ( 'NONE',  ( -7.617292153972128332, 43.16748516956134551, 75.45433879953087342 ) ) ;
#7901 = CARTESIAN_POINT ( 'NONE',  ( 8.317158657711994252, 46.70735294479731436, 78.73595644658969661 ) ) ;
#7902 = ADVANCED_FACE ( 'NONE', ( #8047 ), #14535, .F. ) ;
#7903 = VERTEX_POINT ( 'NONE', #19422 ) ;
#7904 = DIRECTION ( 'NONE',  ( -4.731737692062861008E-17, 0.7071067811865475727, 0.7071067811865475727 ) ) ;
#7905 = EDGE_LOOP ( 'NONE', ( #20554, #6172, #13813, #5532, #3582, #15295, #20649, #5631, #12785, #17662, #5993, #15157 ) ) ;
#7906 = CARTESIAN_POINT ( 'NONE',  ( -3.799298760401091268, 51.89000185047994052, 75.54713691134779197 ) ) ;
#7907 = CARTESIAN_POINT ( 'NONE',  ( -0.3080929418689875576, 37.85583172076933778, 95.10183880123796030 ) ) ;
#7908 = CARTESIAN_POINT ( 'NONE',  ( -7.785425530191283805, 41.22750551581724210, 78.59694605312716931 ) ) ;
#7909 = VERTEX_POINT ( 'NONE', #3258 ) ;
#7910 = PLANE ( 'NONE',  #18108 ) ;
#7911 = DIRECTION ( 'NONE',  ( 1.334402673828313339E-16, 1.871524341742854397E-32, -1.000000000000000000 ) ) ;
#7912 = AXIS2_PLACEMENT_3D ( 'NONE', #8118, #14501, #135 ) ;
#7913 = DIRECTION ( 'NONE',  ( 3.893792155548169402E-16, 7.183611964723547524E-17, -1.000000000000000000 ) ) ;
#7914 = ADVANCED_FACE ( 'NONE', ( #10074 ), #14745, .F. ) ;
#7915 = CARTESIAN_POINT ( 'NONE',  ( 5.200734800563608928, 50.89208066999871249, 76.39036821129558064 ) ) ;
#7916 = CARTESIAN_POINT ( 'NONE',  ( 0.5221537403064990812, 44.16218137147969003, 95.05433879953096721 ) ) ;
#7917 = VERTEX_POINT ( 'NONE', #9757 ) ;
#7918 = FACE_OUTER_BOUND ( 'NONE', #3826, .T. ) ;
#7919 = FACE_OUTER_BOUND ( 'NONE', #20305, .T. ) ;
#7920 = ADVANCED_FACE ( 'NONE', ( #17934 ), #8364, .T. ) ;
#7921 = VERTEX_POINT ( 'NONE', #66 ) ;
#7922 = CARTESIAN_POINT ( 'NONE',  ( 0.8855318251337070956, 49.43213155335586606, 95.05433879953096721 ) ) ;
#7923 = CARTESIAN_POINT ( 'NONE',  ( 4.787119196602786175, 47.27648799119742051, 95.05433879953092458 ) ) ;
#7924 = CARTESIAN_POINT ( 'NONE',  ( -5.838369852643723767, 50.43295630312090339, 76.72345405564152543 ) ) ;
#7925 = CARTESIAN_POINT ( 'NONE',  ( -1.187946976321871073, 48.86064447540922373, 91.54808879611698558 ) ) ;
#7926 = CARTESIAN_POINT ( 'NONE',  ( -1.419351766502866541, 49.49642391118513274, 91.00121379782397923 ) ) ;
#7927 = EDGE_CURVE ( 'NONE', #15976, #15529, #1960, .T. ) ;
#7928 =( BOUNDED_SURFACE ( )  B_SPLINE_SURFACE ( 1, 2, ( 
 ( #19623, #1873, #10175, #3460, #6645, #2079, #8361, #14842, #13670, #12401, #7171, #5675, #18778, #9099, #17079, #20469, #18880, #15588, #9212, #2705, #2395, #8998, #20145, #10611, #1004, #15699, #797, #5577, #4288, #12081, #7281, #2505, #20356, #18562, #15485, #5904, #18663, #5794, #4084, #896, #3975, #7384, #1117, #10500, #13772, #10814, #17280, #692, #16965, #13874, #8897, #15384, #20245, #12186, #12299, #10720, #4193, #17179, #2603, #7499, #13987, #539, #18420, #2040, #19797, #13324, #5218, #7020, #10248, #13631, #6923, #15129, #441, #18307, #3528, #13427, #15343, #1931, #3627, #10465, #20106 ),
 ( #10033, #5426, #19895, #18109, #11632, #8855, #327, #16619, #11734, #8426, #16515, #16831, #8649, #13521, #2248, #16930, #18207, #5113, #14904, #5317, #6818, #11833, #10137, #3728, #757, #8536, #15023, #16725, #2149, #3839, #3941, #19994, #2353, #11943, #5544, #10360, #8747, #12050, #18527, #15234, #648, #7130, #7243, #19691, #20537, #7671, #15662, #2883, #1281, #14147, #2466, #4354, #17040, #5752, #7569, #14051, #2781, #9063, #9282, #10879, #15551, #9380, #19056, #13738, #20209, #968, #17352, #12260, #15772, #1183, #7346, #7456, #15867, #2668, #5641, #8961, #10987, #13953, #20434, #12151, #5863 ) ),
 .UNSPECIFIED., .F., .F., .F. ) 
 B_SPLINE_SURFACE_WITH_KNOTS ( ( 2, 2 ),
 ( 3, 2, 2, 2, 2, 2, 2, 2, 2, 2, 2, 2, 2, 2, 2, 2, 2, 2, 2, 2, 2, 2, 2, 2, 2, 2, 2, 2, 2, 2, 2, 2, 2, 2, 2, 2, 2, 2, 2, 2, 3 ),
 ( 0.000000000000000000, 1.000000000000000000 ),
 ( 0.000000000000000000, 0.02500000000000000139, 0.05000000000000000278, 0.07499999999999999722, 0.1000000000000000056, 0.1250000000000000000, 0.1499999999999999944, 0.1749999999999999889, 0.2000000000000000111, 0.2250000000000000056, 0.2500000000000000000, 0.2750000000000000222, 0.2999999999999999889, 0.3250000000000000111, 0.3499999999999999778, 0.3750000000000000000, 0.4000000000000000222, 0.4249999999999999889, 0.4500000000000000111, 0.4749999999999999778, 0.5000000000000000000, 0.5250000000000000222, 0.5500000000000000444, 0.5749999999999999556, 0.5999999999999999778, 0.6250000000000000000, 0.6500000000000000222, 0.6750000000000000444, 0.6999999999999999556, 0.7249999999999999778, 0.7500000000000000000, 0.7750000000000000222, 0.8000000000000000444, 0.8249999999999999556, 0.8499999999999999778, 0.8750000000000000000, 0.9000000000000000222, 0.9250000000000000444, 0.9499999999999999556, 0.9600309411673831894, 0.9696312505790569691 ),
 .UNSPECIFIED. ) 
 GEOMETRIC_REPRESENTATION_ITEM ( )  RATIONAL_B_SPLINE_SURFACE ( (
 ( 1.000000000000000000, 0.9238795325112867385, 1.000000000000000000, 0.9238795325112867385, 1.000000000000000000, 0.9238795325112867385, 1.000000000000000000, 0.9238795325112867385, 1.000000000000000000, 0.9238795325112867385, 1.000000000000000000, 0.9238795325112867385, 1.000000000000000000, 0.9238795325112867385, 1.000000000000000000, 0.9238795325112867385, 1.000000000000000000, 0.9238795325112867385, 1.000000000000000000, 0.9238795325112867385, 1.000000000000000000, 0.9238795325112867385, 1.000000000000000000, 0.9238795325112867385, 1.000000000000000000, 0.9238795325112867385, 1.000000000000000000, 0.9238795325112867385, 1.000000000000000000, 0.9238795325112867385, 1.000000000000000000, 0.9238795325112867385, 1.000000000000000000, 0.9238795325112867385, 1.000000000000000000, 0.9238795325112867385, 1.000000000000000000, 0.9238795325112867385, 1.000000000000000000, 0.9238795325112867385, 1.000000000000000000, 0.9238795325112867385, 1.000000000000000000, 0.9238795325112867385, 1.000000000000000000, 0.9238795325112867385, 1.000000000000000000, 0.9238795325112867385, 1.000000000000000000, 0.9238795325112867385, 1.000000000000000000, 0.9238795325112867385, 1.000000000000000000, 0.9238795325112867385, 1.000000000000000000, 0.9238795325112867385, 1.000000000000000000, 0.9238795325112867385, 1.000000000000000000, 0.9238795325112867385, 1.000000000000000000, 0.9238795325112867385, 1.000000000000000000, 0.9238795325112867385, 1.000000000000000000, 0.9238795325112867385, 1.000000000000000000, 0.9238795325112867385, 1.000000000000000000, 0.9238795325112867385, 1.000000000000000000, 0.9238795325112867385, 1.000000000000000000, 0.9238795325112867385, 1.000000000000000000, 0.9238795325112867385, 1.000000000000000000, 0.9694576027594803413, 0.9634247247054007479, 0.9634247247054007479, 0.9634247247054007479),
 ( 1.000000000000000000, 0.9238795325112867385, 1.000000000000000000, 0.9238795325112867385, 1.000000000000000000, 0.9238795325112867385, 1.000000000000000000, 0.9238795325112867385, 1.000000000000000000, 0.9238795325112867385, 1.000000000000000000, 0.9238795325112867385, 1.000000000000000000, 0.9238795325112867385, 1.000000000000000000, 0.9238795325112867385, 1.000000000000000000, 0.9238795325112867385, 1.000000000000000000, 0.9238795325112867385, 1.000000000000000000, 0.9238795325112867385, 1.000000000000000000, 0.9238795325112867385, 1.000000000000000000, 0.9238795325112867385, 1.000000000000000000, 0.9238795325112867385, 1.000000000000000000, 0.9238795325112867385, 1.000000000000000000, 0.9238795325112867385, 1.000000000000000000, 0.9238795325112867385, 1.000000000000000000, 0.9238795325112867385, 1.000000000000000000, 0.9238795325112867385, 1.000000000000000000, 0.9238795325112867385, 1.000000000000000000, 0.9238795325112867385, 1.000000000000000000, 0.9238795325112867385, 1.000000000000000000, 0.9238795325112867385, 1.000000000000000000, 0.9238795325112867385, 1.000000000000000000, 0.9238795325112867385, 1.000000000000000000, 0.9238795325112867385, 1.000000000000000000, 0.9238795325112867385, 1.000000000000000000, 0.9238795325112867385, 1.000000000000000000, 0.9238795325112867385, 1.000000000000000000, 0.9238795325112867385, 1.000000000000000000, 0.9238795325112867385, 1.000000000000000000, 0.9238795325112867385, 1.000000000000000000, 0.9238795325112867385, 1.000000000000000000, 0.9238795325112867385, 1.000000000000000000, 0.9238795325112867385, 1.000000000000000000, 0.9238795325112867385, 1.000000000000000000, 0.9238795325112867385, 1.000000000000000000, 0.9238795325112867385, 1.000000000000000000, 0.9694576027594803413, 0.9634247247054007479, 0.9634247247054007479, 0.9634247247054007479) ) ) 
 REPRESENTATION_ITEM ( '' )  SURFACE ( )  );
#7930 = EDGE_CURVE ( 'NONE', #6620, #16858, #9865, .T. ) ;
#7929 = CYLINDRICAL_SURFACE ( 'NONE', #1698, 6.000000000000001776 ) ;
#7931 = EDGE_CURVE ( 'NONE', #19935, #10420, #6649, .T. ) ;
#7932 = VECTOR ( 'NONE', #5537, 1000.000000000000000 ) ;
#7933 = CARTESIAN_POINT ( 'NONE',  ( 5.740585635973908474, 51.24795054640212300, 75.97198585835440099 ) ) ;
#7934 = ORIENTED_EDGE ( 'NONE', *, *, #11800, .T. ) ;
#7935 = CARTESIAN_POINT ( 'NONE',  ( -7.014601640787291537, 47.39335580518124402, 78.31172685814304657 ) ) ;
#7936 = ORIENTED_EDGE ( 'NONE', *, *, #8042, .T. ) ;
#7937 = CARTESIAN_POINT ( 'NONE',  ( -2.917199766949189588, 51.60602765227618960, 76.69845644658968808 ) ) ;
#7938 = EDGE_CURVE ( 'NONE', #17046, #19575, #14845, .T. ) ;
#7939 = DIRECTION ( 'NONE',  ( -0.007885122365278605591, -0.9999689119394085113, -1.805443505845548073E-16 ) ) ;
#7940 = CARTESIAN_POINT ( 'NONE',  ( 9.347650859976274873, 42.80922713344904196, 78.67881838835081965 ) ) ;
#7941 = CARTESIAN_POINT ( 'NONE',  ( 8.034263824280252209, 41.23734091826108283, 79.52393066155629242 ) ) ;
#7942 = ORIENTED_EDGE ( 'NONE', *, *, #10188, .F. ) ;
#7943 = DIRECTION ( 'NONE',  ( 0.5941461771851693774, 0.8043570849667760481, 2.357623395011396791E-16 ) ) ;
#7944 = ORIENTED_EDGE ( 'NONE', *, *, #18034, .F. ) ;
#7945 = CARTESIAN_POINT ( 'NONE',  ( -3.538420156175611897, 36.22114913392427127, 76.12177974158937843 ) ) ;
#7946 = CARTESIAN_POINT ( 'NONE',  ( -4.171401865331652026, 37.44334316642215299, 76.17409373158149322 ) ) ;
#7947 = CARTESIAN_POINT ( 'NONE',  ( 4.987494971863720927, 47.58855820898865829, 95.96121379953099506 ) ) ;
#7948 = ORIENTED_EDGE ( 'NONE', *, *, #13380, .T. ) ;
#7949 = CARTESIAN_POINT ( 'NONE',  ( -4.850396850989176833, 37.19025346873809212, 77.31947969467269388 ) ) ;
#7950 = DIRECTION ( 'NONE',  ( -1.110223024625156540E-16, -1.000000000000000000, -5.922860397471808077E-17 ) ) ;
#7951 = CARTESIAN_POINT ( 'NONE',  ( 2.921181103050040306, 49.30691215337508737, 90.84496379782399345 ) ) ;
#7952 = VECTOR ( 'NONE', #10647, 1000.000000000000227 ) ;
#7953 = EDGE_LOOP ( 'NONE', ( #14416, #12168, #8050, #9492 ) ) ;
#7954 = CARTESIAN_POINT ( 'NONE',  ( 2.263811127080452845, 49.90383875825364157, 77.41268141275706682 ) ) ;
#7955 = FACE_OUTER_BOUND ( 'NONE', #14015, .T. ) ;
#7956 = CARTESIAN_POINT ( 'NONE',  ( 3.460444912181559474, 49.25145096859824889, 93.14871380123798872 ) ) ;
#7957 =( NAMED_UNIT ( * ) SI_UNIT ( $, .STERADIAN. ) SOLID_ANGLE_UNIT ( ) );
#7958 = CARTESIAN_POINT ( 'NONE',  ( -5.706182906969134550, 50.52741225482698439, 75.88700421999355683 ) ) ;
#7959 = DIRECTION ( 'NONE',  ( 0.5813877811927011807, -0.8136266022444372803, -5.636455622144619183E-17 ) ) ;
#7960 = CARTESIAN_POINT ( 'NONE',  ( 8.863132018971368709, 41.35709342965520818, 77.52392363563762956 ) ) ;
#7961 = ADVANCED_FACE ( 'NONE', ( #14951 ), #19834, .F. ) ;
#7962 = EDGE_LOOP ( 'NONE', ( #5705, #20672, #10480, #10837 ) ) ;
#7963 = LINE ( 'NONE', #14447, #8133 ) ;
#7964 = CARTESIAN_POINT ( 'NONE',  ( -0.9346256470065343880, 52.97985314436952820, 78.20877650441246942 ) ) ;
#7965 = ORIENTED_EDGE ( 'NONE', *, *, #6746, .T. ) ;
#7966 = LINE ( 'NONE', #4646, #5068 ) ;
#7967 = CARTESIAN_POINT ( 'NONE',  ( 8.642115653336615466, 43.05911141134401277, 76.45750776978282204 ) ) ;
#7968 = ADVANCED_FACE ( 'NONE', ( #5255 ), #372, .F. ) ;
#7969 = CARTESIAN_POINT ( 'NONE',  ( 8.479137094719348511, 40.20623628148813111, 79.16795596456493911 ) ) ;
#7970 = CARTESIAN_POINT ( 'NONE',  ( 6.920970967149330910, 50.37604745108433946, 78.34373887323252461 ) ) ;
#7971 = ORIENTED_EDGE ( 'NONE', *, *, #16993, .F. ) ;
#7972 = ORIENTED_EDGE ( 'NONE', *, *, #2390, .T. ) ;
#7973 = CARTESIAN_POINT ( 'NONE',  ( 5.184346195548518388, 46.85389944066486123, 93.74612681657400515 ) ) ;
#7974 = FACE_OUTER_BOUND ( 'NONE', #8705, .T. ) ;
#7975 = PLANE ( 'NONE',  #7212 ) ;
#7976 = EDGE_CURVE ( 'NONE', #2983, #5644, #19627, .T. ) ;
#7977 = CARTESIAN_POINT ( 'NONE',  ( 5.120163643319172841, 50.95392860687110925, 79.53967584612604469 ) ) ;
#7978 = LINE ( 'NONE', #7871, #450 ) ;
#7979 = FACE_OUTER_BOUND ( 'NONE', #8826, .T. ) ;
#7980 = CARTESIAN_POINT ( 'NONE',  ( 6.444701727025162974, 49.83360289536132370, 78.07866327931512274 ) ) ;
#7981 = DIRECTION ( 'NONE',  ( -1.110223024625156540E-16, -1.000000000000000000, -5.922860397471808077E-17 ) ) ;
#7982 = CARTESIAN_POINT ( 'NONE',  ( -7.075244453723417593, 44.52209897503762193, 72.45433879953085921 ) ) ;
#7983 = LINE ( 'NONE', #10773, #9470 ) ;
#7984 = CARTESIAN_POINT ( 'NONE',  ( -7.677846259693481556, 40.96218137147969429, 45.55433879953098852 ) ) ;
#7985 = ORIENTED_EDGE ( 'NONE', *, *, #11092, .T. ) ;
#7986 = CARTESIAN_POINT ( 'NONE',  ( 8.814092166714756260, 41.21011788141189669, 78.88950904781501094 ) ) ;
#7987 = CARTESIAN_POINT ( 'NONE',  ( 5.665287683258889651, 37.02150436742986273, 75.36022115247205022 ) ) ;
#7988 = CARTESIAN_POINT ( 'NONE',  ( -3.056480504853190894, 36.78428345565664159, 76.74165022305851380 ) ) ;
#7989 = ORIENTED_EDGE ( 'NONE', *, *, #3915, .T. ) ;
#7990 = LINE ( 'NONE', #12570, #8524 ) ;
#7991 = CARTESIAN_POINT ( 'NONE',  ( 8.395197883163783459, 39.95466513945179798, 76.21925085218815354 ) ) ;
#7992 = ORIENTED_EDGE ( 'NONE', *, *, #12976, .T. ) ;
#7993 = CARTESIAN_POINT ( 'NONE',  ( -0.2542917792799709864, 52.21406978104435836, 75.49651412033875886 ) ) ;
#7994 = CARTESIAN_POINT ( 'NONE',  ( -4.574316323987747346, 51.33620267474496757, 79.54845644658969661 ) ) ;
#7995 = CARTESIAN_POINT ( 'NONE',  ( 7.686414200152805520, 40.17302391697257491, 78.47632680691248197 ) ) ;
#7996 = CARTESIAN_POINT ( 'NONE',  ( 0.6802164782827634371, 52.96490953415155190, 75.98308111960244560 ) ) ;
#7997 = DIRECTION ( 'NONE',  ( 1.000000000000000000, 1.213411507412056509E-16, -0.000000000000000000 ) ) ;
#7998 = ORIENTED_EDGE ( 'NONE', *, *, #17843, .T. ) ;
#7999 = CARTESIAN_POINT ( 'NONE',  ( -4.598246518171406727, 51.31910303412164609, 78.93669174070734584 ) ) ;
#8000 = VERTEX_POINT ( 'NONE', #16243 ) ;
#8001 = CARTESIAN_POINT ( 'NONE',  ( 2.043125170982144745, 38.48583871533720213, 95.02371380123798872 ) ) ;
#8002 = CARTESIAN_POINT ( 'NONE',  ( -3.350035803220276609, 49.20851703305431357, 91.97683880123797451 ) ) ;
#8003 = CARTESIAN_POINT ( 'NONE',  ( 4.722153740306502812, 44.16218137147969003, 45.55433879953098852 ) ) ;
#8004 = DIRECTION ( 'NONE',  ( 1.402518428993831676E-16, -1.000000000000000000, 0.000000000000000000 ) ) ;
#8005 = CARTESIAN_POINT ( 'NONE',  ( -7.934068236863534906, 41.70470996953825704, 78.85747680284711691 ) ) ;
#8006 = B_SPLINE_SURFACE_WITH_KNOTS ( 'NONE', 3, 1, ( 
 ( #2161, #3850 ),
 ( #7889, #20548 ),
 ( #5972, #7783 ),
 ( #14264, #4674 ),
 ( #15674, #12473 ),
 ( #17668, #12779 ),
 ( #19260, #1398 ),
 ( #1094, #5880 ),
 ( #11196, #14375 ),
 ( #18852, #6179 ),
 ( #20745, #6278 ) ),
 .UNSPECIFIED., .F., .F., .F.,
 ( 4, 1, 1, 1, 1, 1, 1, 1, 4 ),
 ( 2, 2 ),
 ( 0.000000000000000000, 0.1094333067106434410, 0.2184679721593839052, 0.3300813608894926365, 0.4462978032959263319, 0.5702501687912749917, 0.7022991718047063570, 0.8456887798043180027, 0.9999999999999998890 ),
 ( 0.000000000000000000, 1.000000000000000000 ),
 .UNSPECIFIED. ) ;
#8007 = ORIENTED_EDGE ( 'NONE', *, *, #3657, .T. ) ;
#8008 = CARTESIAN_POINT ( 'NONE',  ( 4.751063331615088536, 51.97887081224218520, 77.86982703766624070 ) ) ;
#8009 = VERTEX_POINT ( 'NONE', #2082 ) ;
#8010 = CARTESIAN_POINT ( 'NONE',  ( 0.8455950101471351177, 52.35579997042385259, 76.48963291717792856 ) ) ;
#8011 = CARTESIAN_POINT ( 'NONE',  ( -4.524181921268124462, 40.28999182795290324, 91.19558880123797451 ) ) ;
#8012 = CARTESIAN_POINT ( 'NONE',  ( 6.198496396448986090, 45.68315280215533392, 95.33621380123798872 ) ) ;
#8013 = ORIENTED_EDGE ( 'NONE', *, *, #8, .F. ) ;
#8014 = CARTESIAN_POINT ( 'NONE',  ( 1.083001295814570053, 52.34297901104275041, 76.77198585835439815 ) ) ;
#8015 = CARTESIAN_POINT ( 'NONE',  ( -1.214884381343054542, 47.76843358786783256, 85.41730067788145675 ) ) ;
#8016 = CARTESIAN_POINT ( 'NONE',  ( -4.621383371311751809, 37.02109043652605180, 78.92211507803222048 ) ) ;
#8017 = CARTESIAN_POINT ( 'NONE',  ( -4.491212578019011303, 51.39558556899189057, 78.91875292420674270 ) ) ;
#8018 = EDGE_CURVE ( 'NONE', #16288, #11321, #3667, .T. ) ;
#8019 = DIRECTION ( 'NONE',  ( -1.290716872006552287E-16, -1.000000000000000000, 0.000000000000000000 ) ) ;
#8020 = VERTEX_POINT ( 'NONE', #16661 ) ;
#8021 = CARTESIAN_POINT ( 'NONE',  ( -4.344483343973046807, 41.29210034554949971, 92.55433879953100984 ) ) ;
#8022 = CARTESIAN_POINT ( 'NONE',  ( -5.531051774427891310, 44.10426199826898142, 72.45432679953087529 ) ) ;
#8023 = ORIENTED_EDGE ( 'NONE', *, *, #12875, .F. ) ;
#8024 = CARTESIAN_POINT ( 'NONE',  ( 4.640492351041169528, 52.06054514152135937, 78.02172882224894579 ) ) ;
#8025 = CYLINDRICAL_SURFACE ( 'NONE', #17999, 8.199999999999999289 ) ;
#8026 = CARTESIAN_POINT ( 'NONE',  ( -7.376743071288318632, 41.96049357349896525, 78.50654468188380974 ) ) ;
#8027 = CARTESIAN_POINT ( 'NONE',  ( -5.396784162528952322, 49.82872168751453756, 76.45423404125398292 ) ) ;
#8028 = CARTESIAN_POINT ( 'NONE',  ( -3.134114116279072881, 48.15229756555780227, 94.12621379611699979 ) ) ;
#8029 = CARTESIAN_POINT ( 'NONE',  ( 5.052198367669454626, 48.31320248322254685, 92.01683879782399345 ) ) ;
#8030 = CARTESIAN_POINT ( 'NONE',  ( -1.047061061252483327, 36.11373028406117669, 72.45433879953085921 ) ) ;
#8031 = DIRECTION ( 'NONE',  ( 1.540237394707284220E-16, 1.793354297423764243E-16, -1.000000000000000000 ) ) ;
#8032 = VECTOR ( 'NONE', #6052, 1000.000000000000114 ) ;
#8033 = CARTESIAN_POINT ( 'NONE',  ( -3.080034802530627225, 36.80739128506166224, 77.14704031750767399 ) ) ;
#8034 = EDGE_CURVE ( 'NONE', #6210, #13018, #8954, .T. ) ;
#8035 = ORIENTED_EDGE ( 'NONE', *, *, #920, .T. ) ;
#8036 = CARTESIAN_POINT ( 'NONE',  ( 1.996851819492591495, 52.20245025342703826, 78.99734963310253022 ) ) ;
#8037 = CARTESIAN_POINT ( 'NONE',  ( -3.755902984582864867, 36.38179493852598512, 77.82155188814751057 ) ) ;
#8038 = ORIENTED_EDGE ( 'NONE', *, *, #4355, .F. ) ;
#8039 = CARTESIAN_POINT ( 'NONE',  ( 0.5221537403065019678, 44.16218137147968292, 72.45433879953087342 ) ) ;
#8040 = CARTESIAN_POINT ( 'NONE',  ( -0.5520076040313395271, 52.29218845565640095, 75.65236789768508174 ) ) ;
#8041 = DIRECTION ( 'NONE',  ( 1.000000000000000000, -1.110223024625156540E-16, 1.779391786395883043E-16 ) ) ;
#8042 = EDGE_CURVE ( 'NONE', #17381, #16609, #6546, .T. ) ;
#8043 = CARTESIAN_POINT ( 'NONE',  ( -3.765753198988803785, 38.37823718693370978, 75.36022115247205022 ) ) ;
#8044 = VERTEX_POINT ( 'NONE', #13261 ) ;
#8045 = CARTESIAN_POINT ( 'NONE',  ( 0.5221537403065005245, 44.16218137147968292, 82.45433879953087342 ) ) ;
#8046 = ORIENTED_EDGE ( 'NONE', *, *, #18961, .F. ) ;
#8047 = FACE_OUTER_BOUND ( 'NONE', #10852, .T. ) ;
#8048 = CARTESIAN_POINT ( 'NONE',  ( 5.581406744796363562, 50.61539444998253856, 72.45433879953087342 ) ) ;
#8049 = CARTESIAN_POINT ( 'NONE',  ( 1.868012774839550749, 39.13936707477651566, 95.57058879953099506 ) ) ;
#8050 = ORIENTED_EDGE ( 'NONE', *, *, #6651, .F. ) ;
#8051 = CARTESIAN_POINT ( 'NONE',  ( -4.790295051490115696, 37.92061980927154963, 77.33669174070733732 ) ) ;
#8052 = FACE_OUTER_BOUND ( 'NONE', #13440, .T. ) ;
#8053 = CARTESIAN_POINT ( 'NONE',  ( 6.660594192354429843, 43.89417127335556046, 91.86058879782397923 ) ) ;
#8054 = VECTOR ( 'NONE', #432, 1000.000000000000000 ) ;
#8055 = VERTEX_POINT ( 'NONE', #18149 ) ;
#8056 = CARTESIAN_POINT ( 'NONE',  ( -4.592862224480081856, 51.32295045326188898, 75.97198585835440099 ) ) ;
#8057 = DIRECTION ( 'NONE',  ( 0.000000000000000000, 1.000000000000000000, 1.734723475976787846E-14 ) ) ;
#8058 = EDGE_CURVE ( 'NONE', #18072, #17173, #18565, .T. ) ;
#8059 = CARTESIAN_POINT ( 'NONE',  ( 6.102441102155617969, 43.42752260303680600, 89.86746380294499659 ) ) ;
#8060 = CARTESIAN_POINT ( 'NONE',  ( 8.818545868716455516, 41.22346590884859552, 77.48357784852399277 ) ) ;
#8061 = CARTESIAN_POINT ( 'NONE',  ( 5.567302800327750489, 36.95148795754280258, 75.36140480012781495 ) ) ;
#8062 = CARTESIAN_POINT ( 'NONE',  ( -0.7887770423231913464, 52.21626234356678253, 79.01146473771775902 ) ) ;
#8063 = VECTOR ( 'NONE', #17644, 1000.000000000000000 ) ;
#8064 = ORIENTED_EDGE ( 'NONE', *, *, #12013, .F. ) ;
#8065 = PLANE ( 'NONE',  #14598 ) ;
#8066 = FACE_OUTER_BOUND ( 'NONE', #14268, .T. ) ;
#8067 = FACE_BOUND ( 'NONE', #4323, .T. ) ;
#8068 = CARTESIAN_POINT ( 'NONE',  ( 2.119851040271389930, 52.81592988514039178, 78.16610350541323271 ) ) ;
#8069 = VERTEX_POINT ( 'NONE', #3977 ) ;
#8070 = EDGE_CURVE ( 'NONE', #19239, #16089, #11518, .T. ) ;
#8071 = VECTOR ( 'NONE', #7536, 1000.000000000000000 ) ;
#8072 = CARTESIAN_POINT ( 'NONE',  ( 9.271487163511554996, 42.58095970340946934, 75.72637824826109920 ) ) ;
#8074 = ADVANCED_FACE ( 'NONE', ( #7388 ), #13674, .F. ) ;
#8073 = FACE_OUTER_BOUND ( 'NONE', #7429, .T. ) ;
#8075 = DIRECTION ( 'NONE',  ( -1.000000000000000000, 0.000000000000000000, 0.000000000000000000 ) ) ;
#8076 = FACE_OUTER_BOUND ( 'NONE', #111, .T. ) ;
#8077 = DIRECTION ( 'NONE',  ( 1.000000000000000000, 0.000000000000000000, -0.000000000000000000 ) ) ;
#8078 = VECTOR ( 'NONE', #8660, 1000.000000000000000 ) ;
#8079 = CARTESIAN_POINT ( 'NONE',  ( 0.3286341997476255883, 52.35989755568506610, 77.71750713863309556 ) ) ;
#8080 = CARTESIAN_POINT ( 'NONE',  ( 6.174124403209278356, 50.00287997606557155, 77.65065976741861675 ) ) ;
#8081 = CARTESIAN_POINT ( 'NONE',  ( 31.07218010054375412, 42.76218137147968434, 70.80574467885102763 ) ) ;
#8082 = CARTESIAN_POINT ( 'NONE',  ( 6.492824329076245959, 49.76746917884374000, 76.18099276316716839 ) ) ;
#8083 = EDGE_CURVE ( 'NONE', #18535, #2175, #13560, .T. ) ;
#8084 = EDGE_CURVE ( 'NONE', #20802, #18903, #5796, .T. ) ;
#8085 = CARTESIAN_POINT ( 'NONE',  ( 1.352400422481993658, 50.46853102219002096, 93.07058880123798872 ) ) ;
#8086 = ORIENTED_EDGE ( 'NONE', *, *, #2166, .F. ) ;
#8087 = CARTESIAN_POINT ( 'NONE',  ( 8.804944317620233107, 41.18270119734690837, 78.86399424569901839 ) ) ;
#8088 = EDGE_CURVE ( 'NONE', #2266, #799, #17093, .T. ) ;
#8089 = CIRCLE ( 'NONE', #13868, 6.999999999999999112 ) ;
#8090 = CARTESIAN_POINT ( 'NONE',  ( 8.949064546045571333, 41.61463866475444462, 78.77153038569251464 ) ) ;
#8091 = CARTESIAN_POINT ( 'NONE',  ( 5.746684213116473039, 37.07966734754892713, 78.33482135361461474 ) ) ;
#8092 = CARTESIAN_POINT ( 'NONE',  ( 8.119551934336415755, 43.80226376792169418, 72.45433879953087342 ) ) ;
#8093 = CARTESIAN_POINT ( 'NONE',  ( -1.440187084481231006, 38.28092143101017797, 72.45433879953087342 ) ) ;
#8094 = ORIENTED_EDGE ( 'NONE', *, *, #17420, .F. ) ;
#8095 = CARTESIAN_POINT ( 'NONE',  ( -0.4650336042545967219, 52.97492497816961077, 75.60318094692254931 ) ) ;
#8096 = DIRECTION ( 'NONE',  ( -1.334402673828316297E-16, 2.168404344970984808E-15, 1.000000000000000000 ) ) ;
#8097 = CARTESIAN_POINT ( 'NONE',  ( 6.446960153690390882, 38.49983447822285143, 77.31245045813156480 ) ) ;
#8098 = DIRECTION ( 'NONE',  ( 0.000000000000000000, 1.000000000000000000, 0.000000000000000000 ) ) ;
#8099 = DIRECTION ( 'NONE',  ( 1.540237394707284220E-16, 1.793354297423764243E-16, -1.000000000000000000 ) ) ;
#8100 = ORIENTED_EDGE ( 'NONE', *, *, #2607, .F. ) ;
#8101 = CARTESIAN_POINT ( 'NONE',  ( -1.123656915330052408, 35.37488560990637865, 76.16022115247204738 ) ) ;
#8102 = CIRCLE ( 'NONE', #7771, 4.199999999999999289 ) ;
#8103 = VERTEX_POINT ( 'NONE', #2398 ) ;
#8104 = CARTESIAN_POINT ( 'NONE',  ( 2.043125170982144745, 38.48583871533720213, 91.27371380123798872 ) ) ;
#8105 = ADVANCED_FACE ( 'NONE', ( #15165 ), #10398, .T. ) ;
#8106 = CARTESIAN_POINT ( 'NONE',  ( 1.167393906761340361, 52.20907389968696322, 76.77301385304936332 ) ) ;
#8107 = CARTESIAN_POINT ( 'NONE',  ( 5.843112203128086435, 37.14857125875717969, 76.21413800766271152 ) ) ;
#8108 = DIRECTION ( 'NONE',  ( -1.540237394707284467E-16, -1.793354297423764243E-16, 1.000000000000000000 ) ) ;
#8109 = DIRECTION ( 'NONE',  ( -1.000000000000000000, -1.402518428993831676E-16, -1.196361017915039239E-16 ) ) ;
#8110 = ORIENTED_EDGE ( 'NONE', *, *, #4789, .T. ) ;
#8111 = CARTESIAN_POINT ( 'NONE',  ( -4.532046673723619357, 36.95510101671939651, 76.17409373158149322 ) ) ;
#8112 = VECTOR ( 'NONE', #4154, 1000.000000000000000 ) ;
#8113 = ORIENTED_EDGE ( 'NONE', *, *, #1283, .T. ) ;
#8114 = LINE ( 'NONE', #1525, #5428 ) ;
#8115 = CARTESIAN_POINT ( 'NONE',  ( 5.568489401881125289, 48.03437091500646261, 90.57058880123798872 ) ) ;
#8116 = CARTESIAN_POINT ( 'NONE',  ( 3.460444912181559474, 49.25145096859824889, 94.24246380123798872 ) ) ;
#8117 = VERTEX_POINT ( 'NONE', #12188 ) ;
#8118 = CARTESIAN_POINT ( 'NONE',  ( 27.03948732994508930, 45.16218137147969003, 76.90433879953101837 ) ) ;
#8119 = CARTESIAN_POINT ( 'NONE',  ( -3.349688636638950889, 52.21127678364309332, 78.10580938776615767 ) ) ;
#8120 = CARTESIAN_POINT ( 'NONE',  ( -4.030157702633147210, 50.97812307042602953, 78.45066232894264147 ) ) ;
#8121 = CARTESIAN_POINT ( 'NONE',  ( 5.427780505986065762, 36.85179043424346190, 77.43080938776617472 ) ) ;
#8122 = ORIENTED_EDGE ( 'NONE', *, *, #20735, .T. ) ;
#8123 = DIRECTION ( 'NONE',  ( -0.8134066734386236064, -0.5812306281201740088, 0.02324952774876324485 ) ) ;
#8124 = DIRECTION ( 'NONE',  ( 0.3014925587070406698, -0.9534141535609406137, 0.01018277142809568582 ) ) ;
#8125 = EDGE_LOOP ( 'NONE', ( #7391, #10201, #13777, #10916 ) ) ;
#8126 = CARTESIAN_POINT ( 'NONE',  ( -1.692449145443465808, 49.14138036605904603, 95.05433879953098142 ) ) ;
#8127 = CARTESIAN_POINT ( 'NONE',  ( -4.517072128342571880, 36.94403992325788977, 78.58080938776616620 ) ) ;
#8128 = VECTOR ( 'NONE', #19706, 1000.000000000000000 ) ;
#8129 = CARTESIAN_POINT ( 'NONE',  ( -4.735834763901007882, 50.30101192887209294, 75.43678921887351407 ) ) ;
#8130 = CARTESIAN_POINT ( 'NONE',  ( 0.7582201636353278484, 49.56899138526064519, 93.96996379611699979 ) ) ;
#8131 = PLANE ( 'NONE',  #16445 ) ;
#8132 = DIRECTION ( 'NONE',  ( 1.540237394707284220E-16, 1.793354297423764243E-16, -1.000000000000000000 ) ) ;
#8133 = VECTOR ( 'NONE', #19136, 1000.000000000000000 ) ;
#8134 = CARTESIAN_POINT ( 'NONE',  ( 5.904402762709062280, 51.12694543383925350, 76.06909773771320715 ) ) ;
#8135 = B_SPLINE_CURVE_WITH_KNOTS ( 'NONE', 3,
 ( #11713, #14882, #18284, #6798, #3506, #6901, #6993, #13403, #3816, #13303, #1911, #19775, #14997, #18187 ),
 .UNSPECIFIED., .F., .F.,
 ( 4, 2, 2, 2, 2, 2, 4 ),
 ( 0.000000000000000000, 0.0006024534355434134824, 0.0009036801533151169168, 0.001204906871086820460, 0.001506133588858523569, 0.001807360306630227328, 0.002409813742173637016 ),
 .UNSPECIFIED. ) ;
#8136 = EDGE_LOOP ( 'NONE', ( #7705, #5771, #1626, #16118 ) ) ;
#8137 = FACE_OUTER_BOUND ( 'NONE', #13231, .T. ) ;
#8138 = EDGE_CURVE ( 'NONE', #1661, #20573, #2285, .T. ) ;
#8139 = VECTOR ( 'NONE', #16869, 1000.000000000000227 ) ;
#8140 = CARTESIAN_POINT ( 'NONE',  ( -3.555031842569258416, 52.06454604677990972, 75.79042024895623797 ) ) ;
#8141 = EDGE_LOOP ( 'NONE', ( #1993, #18742, #987, #3195, #7335, #12561, #2584, #6317, #8773, #17058, #19617, #6657, #17634, #7465, #3573, #10524, #9347, #9263, #18451 ) ) ;
#8142 = LINE ( 'NONE', #16451, #7540 ) ;
#8143 = DIRECTION ( 'NONE',  ( 1.402518428993831676E-16, -1.000000000000000000, 0.000000000000000000 ) ) ;
#8144 = EDGE_LOOP ( 'NONE', ( #12012, #6096, #2695, #10400 ) ) ;
#8145 = AXIS2_PLACEMENT_3D ( 'NONE', #4021, #2546, #4338 ) ;
#8146 = DIRECTION ( 'NONE',  ( -0.2908163624019201587, 0.9196526680133400022, -0.2639409281927689310 ) ) ;
#8147 = CARTESIAN_POINT ( 'NONE',  ( 5.561379608955574483, 51.38032281970146897, 76.39036821129558064 ) ) ;
#8148 = ORIENTED_EDGE ( 'NONE', *, *, #8177, .F. ) ;
#8149 = CARTESIAN_POINT ( 'NONE',  ( 5.599463258324014703, 51.35219196201597214, 78.62371398036725623 ) ) ;
#8150 = DIRECTION ( 'NONE',  ( 1.540237394707284220E-16, 1.793354297423764243E-16, -1.000000000000000000 ) ) ;
#8151 = CARTESIAN_POINT ( 'NONE',  ( 5.544968037009670780, 45.50804040601273925, 94.63308879953099506 ) ) ;
#8152 = VERTEX_POINT ( 'NONE', #7286 ) ;
#8153 = CARTESIAN_POINT ( 'NONE',  ( -4.529265440370444651, 36.95304663167630821, 77.01245883157920957 ) ) ;
#8154 = CARTESIAN_POINT ( 'NONE',  ( -4.990412171993382273, 37.29367714620268259, 77.90250793075740887 ) ) ;
#8155 = EDGE_CURVE ( 'NONE', #19085, #5478, #19933, .T. ) ;
#8156 = AXIS2_PLACEMENT_3D ( 'NONE', #10535, #15419, #3697 ) ;
#8157 = ORIENTED_EDGE ( 'NONE', *, *, #10247, .T. ) ;
#8158 = CARTESIAN_POINT ( 'NONE',  ( -4.718161399584266391, 37.09257646755418847, 75.97198585835440099 ) ) ;
#8159 = DIRECTION ( 'NONE',  ( -1.002887009549092588E-15, -1.000000000000000000, 0.000000000000000000 ) ) ;
#8160 = LINE ( 'NONE', #485, #9859 ) ;
#8161 = CARTESIAN_POINT ( 'NONE',  ( 1.256812508749381774, 49.74246873332880625, 90.17996380294496817 ) ) ;
#8162 = CIRCLE ( 'NONE', #5427, 4.200000000000001066 ) ;
#8163 = VECTOR ( 'NONE', #11740, 1000.000000000000000 ) ;
#8164 = CARTESIAN_POINT ( 'NONE',  ( 0.6135150644279553367, 52.34298826783862779, 76.85126224504509196 ) ) ;
#8165 = DIRECTION ( 'NONE',  ( 1.540237394707283727E-16, 1.793354297423763257E-16, -1.000000000000000000 ) ) ;
#8166 = CARTESIAN_POINT ( 'NONE',  ( 8.604143167063659448, 40.58088741054138637, 79.41216397796385706 ) ) ;
#8167 = AXIS2_PLACEMENT_3D ( 'NONE', #11816, #8195, #3201 ) ;
#8168 = ORIENTED_EDGE ( 'NONE', *, *, #1045, .F. ) ;
#8169 = CARTESIAN_POINT ( 'NONE',  ( -5.510796958474739604, 38.60848837797752964, 76.73301527011911105 ) ) ;
#8170 = CARTESIAN_POINT ( 'NONE',  ( 8.643862584933666326, 43.06434707616365642, 76.70850639745313515 ) ) ;
#8171 = FACE_OUTER_BOUND ( 'NONE', #14492, .T. ) ;
#8172 = FACE_OUTER_BOUND ( 'NONE', #289, .T. ) ;
#8173 = VERTEX_POINT ( 'NONE', #11873 ) ;
#8174 = CARTESIAN_POINT ( 'NONE',  ( 0.5221537403064985261, 44.16218137147969003, 96.05433879953096721 ) ) ;
#8175 = AXIS2_PLACEMENT_3D ( 'NONE', #10982, #18625, #10772 ) ;
#8176 = ORIENTED_EDGE ( 'NONE', *, *, #19493, .F. ) ;
#8177 = EDGE_CURVE ( 'NONE', #11143, #6944, #2237, .T. ) ;
#8178 = CARTESIAN_POINT ( 'NONE',  ( -1.214884381343048991, 47.76843358786783256, 53.41730067788145675 ) ) ;
#8179 = CARTESIAN_POINT ( 'NONE',  ( 5.453344025566022601, 40.65105419805430387, 72.45432679953087529 ) ) ;
#8180 = CARTESIAN_POINT ( 'NONE',  ( 6.712139372526147341, 50.53030293778272863, 77.80505143490314879 ) ) ;
#8181 = CARTESIAN_POINT ( 'NONE',  ( 4.314486539155690359, 51.43278757724892358, 79.13226549199922033 ) ) ;
#8182 = DIRECTION ( 'NONE',  ( -0.9485903129789527988, 0.3165065846431829311, -8.934458285744989980E-17 ) ) ;
#8183 = PLANE ( 'NONE',  #7746 ) ;
#8184 = EDGE_CURVE ( 'NONE', #8117, #188, #10850, .T. ) ;
#8185 = CARTESIAN_POINT ( 'NONE',  ( 8.643718578691984789, 43.06391548032173944, 77.11956464767864361 ) ) ;
#8186 = B_SPLINE_CURVE_WITH_KNOTS ( 'NONE', 3,
 ( #18365, #15500, #2194, #20162, #8693, #15174, #911, #3887, #589, #7071, #11032, #7825, #9116, #14308, #9226, #18994, #12312, #4408, #17195 ),
 .UNSPECIFIED., .F., .F.,
 ( 4, 1, 1, 1, 1, 1, 1, 1, 1, 1, 1, 1, 1, 1, 1, 1, 4 ),
 ( 0.000000000000000000, 0.08150191411353231719, 0.1574413810301363015, 0.2279254944343154510, 0.2925593756674912393, 0.3532811523109508078, 0.4087341836578463616, 0.4609809767707315764, 0.5093835833650265377, 0.5574898171909816735, 0.6095021731789963537, 0.6642568233027335012, 0.7231084493840179706, 0.7857192733158503417, 0.8528940375925012640, 0.9238451209387705809, 1.000000000000000000 ),
 .UNSPECIFIED. ) ;
#8187 = CARTESIAN_POINT ( 'NONE',  ( 1.352400422481993658, 50.46853102219002096, 90.57058880123798872 ) ) ;
#8188 = EDGE_LOOP ( 'NONE', ( #8732, #15032, #9720, #3687 ) ) ;
#8189 = CARTESIAN_POINT ( 'NONE',  ( -5.681413420386579816, 37.80409193316261707, 79.34222993022952153 ) ) ;
#8190 = EDGE_CURVE ( 'NONE', #17974, #20326, #1316, .T. ) ;
#8191 = DIRECTION ( 'NONE',  ( 1.000000000000000000, 1.402518428993831676E-16, 0.000000000000000000 ) ) ;
#8192 = EDGE_CURVE ( 'NONE', #6620, #2983, #7817, .T. ) ;
#8193 = CARTESIAN_POINT ( 'NONE',  ( -4.534577940854813249, 37.71160670378642266, 78.59503622499423159 ) ) ;
#8194 = PRODUCT_DEFINITION ( 'UNKNOWN', '', #8875, #5736 ) ;
#8195 = DIRECTION ( 'NONE',  ( 1.402518428993831183E-16, -1.000000000000000000, 3.469446951953617640E-16 ) ) ;
#8196 = ADVANCED_FACE ( 'NONE', ( #6207 ), #3253, .F. ) ;
#8197 = EDGE_CURVE ( 'NONE', #11013, #14806, #620, .T. ) ;
#8198 = CARTESIAN_POINT ( 'NONE',  ( 8.572560397843592028, 40.48623184761532912, 75.53366564255911442 ) ) ;
#8199 = ORIENTED_EDGE ( 'NONE', *, *, #18817, .T. ) ;
#8200 = VERTEX_POINT ( 'NONE', #16211 ) ;
#8201 = CARTESIAN_POINT ( 'NONE',  ( 6.872381782841294751, 37.88404961645574076, 76.32925572521180868 ) ) ;
#8202 = VECTOR ( 'NONE', #13072, 1000.000000000000000 ) ;
#8203 = CARTESIAN_POINT ( 'NONE',  ( 0.5221537403065079630, 49.16218137147969003, 93.97886871425482980 ) ) ;
#8204 = CARTESIAN_POINT ( 'NONE',  ( 6.870794506624137377, 37.88291540698485704, 77.55645576794258034 ) ) ;
#8205 = DIRECTION ( 'NONE',  ( 5.731934358295347564E-32, -3.469446951953617147E-16, -1.000000000000000000 ) ) ;
#8206 = PLANE ( 'NONE',  #4145 ) ;
#8207 = VERTEX_POINT ( 'NONE', #5125 ) ;
#8208 = CIRCLE ( 'NONE', #12292, 8.199999999999995737 ) ;
#8209 = EDGE_CURVE ( 'NONE', #20868, #3406, #15581, .T. ) ;
#8210 = DIRECTION ( 'NONE',  ( 1.000000000000000000, 0.000000000000000000, 0.000000000000000000 ) ) ;
#8211 = VERTEX_POINT ( 'NONE', #1945 ) ;
#8212 = CARTESIAN_POINT ( 'NONE',  ( -3.350035803220276609, 49.20851703305431357, 90.72683880123797451 ) ) ;
#8213 = CARTESIAN_POINT ( 'NONE',  ( -7.890048607039471307, 46.74575480130646099, 79.45433879953087342 ) ) ;
#8214 = DIRECTION ( 'NONE',  ( -1.779391786395883536E-16, -5.922860397471806844E-17, 1.000000000000000000 ) ) ;
#8215 = CARTESIAN_POINT ( 'NONE',  ( -7.365114186959480058, 41.93575649144190010, 78.75998376317852490 ) ) ;
#8216 = CIRCLE ( 'NONE', #745, 8.199999999999995737 ) ;
#8217 = CARTESIAN_POINT ( 'NONE',  ( 8.642937017325245108, 43.02502337403097243, 78.77838852948787007 ) ) ;
#8218 = VERTEX_POINT ( 'NONE', #13228 ) ;
#8219 = VECTOR ( 'NONE', #6253, 1000.000000000000000 ) ;
#8220 = VERTEX_POINT ( 'NONE', #10046 ) ;
#8221 = CARTESIAN_POINT ( 'NONE',  ( 0.3326973149608336566, 52.96014171822455552, 77.10139762306027933 ) ) ;
#8222 = EDGE_CURVE ( 'NONE', #3298, #5674, #8346, .T. ) ;
#8223 = CARTESIAN_POINT ( 'NONE',  ( 3.961507247562193523, 36.71833509068317625, 76.96022115247204454 ) ) ;
#8224 = B_SPLINE_CURVE_WITH_KNOTS ( 'NONE', 3,
 ( #13178, #2987, #3589, #15980, #6780, #13075 ),
 .UNSPECIFIED., .F., .F.,
 ( 4, 2, 4 ),
 ( 0.000000000000000000, 0.001391361808504449618, 0.002782723617008899235 ),
 .UNSPECIFIED. ) ;
#8225 = PLANE ( 'NONE',  #18656 ) ;
#8226 = ORIENTED_EDGE ( 'NONE', *, *, #6992, .T. ) ;
#8227 = CARTESIAN_POINT ( 'NONE',  ( 8.214799251806553571, 41.32260305165857517, 77.80727997600146750 ) ) ;
#8228 = LINE ( 'NONE', #11430, #16742 ) ;
#8229 = CARTESIAN_POINT ( 'NONE',  ( 4.677786616261469632, 40.19619496325550756, 92.55433879953091036 ) ) ;
#8230 = CARTESIAN_POINT ( 'NONE',  ( -3.350053155021378792, 52.21101631215288563, 78.15066919019970726 ) ) ;
#8231 = CARTESIAN_POINT ( 'NONE',  ( 0.5221537403065019678, 44.16218137147968292, 72.45433879953087342 ) ) ;
#8232 = ORIENTED_EDGE ( 'NONE', *, *, #5979, .T. ) ;
#8233 = CARTESIAN_POINT ( 'NONE',  ( -4.404666252920439895, 51.45742840424412634, 76.10127045261064893 ) ) ;
#8234 = CARTESIAN_POINT ( 'NONE',  ( 11.22215374030650281, 45.56218137147968150, 72.80433879953100984 ) ) ;
#8235 = VECTOR ( 'NONE', #12749, 1000.000000000000114 ) ;
#8236 = ORIENTED_EDGE ( 'NONE', *, *, #17950, .T. ) ;
#8237 = CARTESIAN_POINT ( 'NONE',  ( 4.623413712694776301, 52.07316044369832042, 78.06776350345396054 ) ) ;
#8238 = CARTESIAN_POINT ( 'NONE',  ( -6.807656070979932750, 40.62200040745536711, 77.60658645233600339 ) ) ;
#8239 = VECTOR ( 'NONE', #5106, 1000.000000000000000 ) ;
#8240 =( BOUNDED_CURVE ( )  B_SPLINE_CURVE ( 3, ( #7397, #15395, #4204, #10509 ),
 .UNSPECIFIED., .F., .T. ) 
 B_SPLINE_CURVE_WITH_KNOTS ( ( 4, 4 ),
 ( 5.988669822071447157, 6.577700792287720866 ),
 .UNSPECIFIED. ) 
 CURVE ( )  GEOMETRIC_REPRESENTATION_ITEM ( )  RATIONAL_B_SPLINE_CURVE ( ( 1.000000000000000000, 0.9712952651971045182, 0.9712952651971045182, 1.000000000000000000 ) ) 
 REPRESENTATION_ITEM ( '' )  );
#8241 = CARTESIAN_POINT ( 'NONE',  ( -4.279734250126900896, 37.51515375910477701, 77.24486754123188348 ) ) ;
#8242 = CARTESIAN_POINT ( 'NONE',  ( 4.512269934384614878, 47.81844922806527620, 93.81371379611701400 ) ) ;
#8243 = DIRECTION ( 'NONE',  ( 0.000000000000000000, 0.000000000000000000, -1.000000000000000000 ) ) ;
#8244 = FACE_OUTER_BOUND ( 'NONE', #11900, .T. ) ;
#8245 = CARTESIAN_POINT ( 'NONE',  ( -3.231322013975681973, 36.91914105393552603, 77.52205638859560111 ) ) ;
#8246 = VERTEX_POINT ( 'NONE', #3542 ) ;
#8247 = DIRECTION ( 'NONE',  ( 1.000000000000000000, -4.930380657631323784E-32, 3.893792155548169402E-16 ) ) ;
#8248 = FACE_OUTER_BOUND ( 'NONE', #4484, .T. ) ;
#8249 = ORIENTED_EDGE ( 'NONE', *, *, #6572, .F. ) ;
#8250 = VECTOR ( 'NONE', #14609, 1000.000000000000000 ) ;
#8251 = LINE ( 'NONE', #19727, #13597 ) ;
#8252 = VECTOR ( 'NONE', #6880, 1000.000000000000000 ) ;
#8253 = DIRECTION ( 'NONE',  ( 0.000000000000000000, 0.000000000000000000, 1.000000000000000000 ) ) ;
#8254 = CARTESIAN_POINT ( 'NONE',  ( 8.872773925109784798, 41.38599083402314704, 79.54845644658969661 ) ) ;
#8255 = ORIENTED_EDGE ( 'NONE', *, *, #11209, .F. ) ;
#8256 = CARTESIAN_POINT ( 'NONE',  ( 4.394343283833276104, 39.11584570990505938, 94.00808880123798872 ) ) ;
#8257 = CARTESIAN_POINT ( 'NONE',  ( -5.176219156857807313, 38.36693177725332760, 75.60525969576029581 ) ) ;
#8258 = ORIENTED_EDGE ( 'NONE', *, *, #16774, .F. ) ;
#8259 = CARTESIAN_POINT ( 'NONE',  ( 4.199109002476567376, 47.83913663364971569, 83.28180655319408743 ) ) ;
#8260 = CARTESIAN_POINT ( 'NONE',  ( -7.677846259693483333, 47.36218137147966445, 80.55433879953099563 ) ) ;
#8261 = CARTESIAN_POINT ( 'NONE',  ( -4.500660556396669065, 42.81632233694663370, 96.50808879953099506 ) ) ;
#8262 = ORIENTED_EDGE ( 'NONE', *, *, #17953, .T. ) ;
#8263 = DIRECTION ( 'NONE',  ( 0.5813877811927012917, -0.8136266022444372803, -5.636455622144620416E-17 ) ) ;
#8264 = CARTESIAN_POINT ( 'NONE',  ( -4.799158982053689293, 37.15240611894265044, 77.91201545794896788 ) ) ;
#8265 = CARTESIAN_POINT ( 'NONE',  ( -1.187946976321871961, 48.86064447540922373, 93.11058879953097289 ) ) ;
#8266 = PRODUCT_DEFINITION_CONTEXT ( 'detailed design', #5588, 'design' ) ;
#8267 = VERTEX_POINT ( 'NONE', #6515 ) ;
#8268 = CARTESIAN_POINT ( 'NONE',  ( -10.17784625969349754, 51.36218137147968577, 54.55433879953098852 ) ) ;
#8269 = DIRECTION ( 'NONE',  ( -1.779391786395883783E-16, -5.922860397471806844E-17, 1.000000000000000000 ) ) ;
#8270 = CARTESIAN_POINT ( 'NONE',  ( 27.03948732994508219, 43.16218137147969003, 73.00433879953099847 ) ) ;
#8271 = CARTESIAN_POINT ( 'NONE',  ( -4.524181921268124462, 40.28999182795290324, 93.53933880123797451 ) ) ;
#8272 = VECTOR ( 'NONE', #16687, 1000.000000000000000 ) ;
#8273 = DIRECTION ( 'NONE',  ( 1.000000000000000000, 0.000000000000000000, 0.000000000000000000 ) ) ;
#8274 = CARTESIAN_POINT ( 'NONE',  ( 6.532049803590284753, 50.66332784790530752, 75.53514883118299394 ) ) ;
#8275 = CARTESIAN_POINT ( 'NONE',  ( -4.497902711709205192, 37.67842107594061929, 76.02644968818945870 ) ) ;
#8276 = DIRECTION ( 'NONE',  ( -1.084202172485505420E-16, -1.000000000000000000, 0.000000000000000000 ) ) ;
#8277 = CARTESIAN_POINT ( 'NONE',  ( 4.695664425361702143, 36.32864708750979332, 75.66510065906194882 ) ) ;
#8278 = CARTESIAN_POINT ( 'NONE',  ( 7.769255851728997797, 40.44309521273268615, 79.16795596456493911 ) ) ;
#8279 = ORIENTED_EDGE ( 'NONE', *, *, #17044, .F. ) ;
#8280 = CARTESIAN_POINT ( 'NONE',  ( -5.442413609737339009, 38.53480995828901712, 75.92268755756494159 ) ) ;
#8281 = CARTESIAN_POINT ( 'NONE',  ( -1.856544280600664454, 49.13739387491266086, 94.21485748750063749 ) ) ;
#8282 = LINE ( 'NONE', #3374, #7226 ) ;
#8283 = PLANE ( 'NONE',  #19425 ) ;
#8284 = ORIENTED_EDGE ( 'NONE', *, *, #1633, .T. ) ;
#8285 = AXIS2_PLACEMENT_3D ( 'NONE', #9539, #9427, #6011 ) ;
#8286 = CARTESIAN_POINT ( 'NONE',  ( 35.92215374030650565, 40.96218137147972982, 93.55433879953098142 ) ) ;
#8287 = ORIENTED_EDGE ( 'NONE', *, *, #5720, .F. ) ;
#8288 = DIRECTION ( 'NONE',  ( 0.000000000000000000, 0.000000000000000000, -1.000000000000000000 ) ) ;
#8289 = CARTESIAN_POINT ( 'NONE',  ( 13.32022995165973001, 36.96218137147968719, 92.39963826115175038 ) ) ;
#8290 = CARTESIAN_POINT ( 'NONE',  ( 8.951667845840693971, 41.62244091939069790, 76.38301527011910252 ) ) ;
#8291 = EDGE_CURVE ( 'NONE', #15187, #15788, #7322, .T. ) ;
#8292 = CARTESIAN_POINT ( 'NONE',  ( 0.5221537403065010796, 44.16218137147969003, 77.84651775085080772 ) ) ;
#8293 = CYLINDRICAL_SURFACE ( 'NONE', #2516, 5.199999999999999289 ) ;
#8294 = CARTESIAN_POINT ( 'NONE',  ( -1.477846259693489372, 50.16218137147969713, 50.55433879953100273 ) ) ;
#8295 = B_SPLINE_CURVE_WITH_KNOTS ( 'NONE', 3,
 ( #16174, #8079, #4871, #15459, #12061, #981, #17056, #10588, #13752, #18757 ),
 .UNSPECIFIED., .F., .F.,
 ( 4, 2, 2, 2, 4 ),
 ( 0.000000000000000000, 0.0001324027139890673291, 0.0002648054279781346582, 0.0003972081419672020145, 0.0005296108559562693165 ),
 .UNSPECIFIED. ) ;
#8296 = CARTESIAN_POINT ( 'NONE',  ( 4.097836514301406829, 51.53655020162395317, 76.55090572632929025 ) ) ;
#8297 = DIRECTION ( 'NONE',  ( 0.9999689119394086223, -0.007885122365275665235, 1.526048693634353392E-16 ) ) ;
#8298 = CARTESIAN_POINT ( 'NONE',  ( -4.895412223390203543, 37.22350451100091817, 76.36316342150684022 ) ) ;
#8299 = CARTESIAN_POINT ( 'NONE',  ( -5.154188915835984375, 42.64120994080404614, 92.21121380123797451 ) ) ;
#8300 = ORIENTED_EDGE ( 'NONE', *, *, #19899, .F. ) ;
#8301 = CARTESIAN_POINT ( 'NONE',  ( 0.3279354649297712143, 52.35625736820495035, 76.44919174070734869 ) ) ;
#8302 = B_SPLINE_CURVE_WITH_KNOTS ( 'NONE', 3,
 ( #11874, #19527, #3465, #19628, #167, #16556, #5256, #1976, #13462, #478, #19734, #4942 ),
 .UNSPECIFIED., .F., .F.,
 ( 4, 2, 2, 2, 2, 4 ),
 ( 0.000000000000000000, 0.0002162791450248731536, 0.0004325582900497463071, 0.0006488374350746195420, 0.0007569770075870690344, 0.0008651165800995185267 ),
 .UNSPECIFIED. ) ;
#8303 = EDGE_CURVE ( 'NONE', #8200, #5130, #19595, .T. ) ;
#8304 = CARTESIAN_POINT ( 'NONE',  ( 8.912702722122396892, 41.50565997170561161, 78.91042349786003740 ) ) ;
#8305 = CARTESIAN_POINT ( 'NONE',  ( 8.636008417968735529, 42.97537321702968427, 75.95421592775571185 ) ) ;
#8306 = CARTESIAN_POINT ( 'NONE',  ( -4.032264951078912141, 50.98107207184723677, 72.45433879953087342 ) ) ;
#8307 = EDGE_CURVE ( 'NONE', #19372, #15205, #8102, .T. ) ;
#8308 = CARTESIAN_POINT ( 'NONE',  ( -5.838428831739583380, 50.43291415881836315, 78.10580938776615767 ) ) ;
#8309 = EDGE_LOOP ( 'NONE', ( #15812, #6395, #18426, #6518, #19654, #9121, #8328, #4518 ) ) ;
#8310 = EDGE_LOOP ( 'NONE', ( #9894, #16453, #10783, #1798 ) ) ;
#8311 = CARTESIAN_POINT ( 'NONE',  ( 6.658811665516601863, 37.73144022991658630, 75.70392102816973079 ) ) ;
#8312 = CARTESIAN_POINT ( 'NONE',  ( -0.1077981546206782937, 52.97333330572794807, 79.46489189366771200 ) ) ;
#8313 = DIRECTION ( 'NONE',  ( -2.267473790562806848E-16, 5.922860397471811774E-17, -1.000000000000000000 ) ) ;
#8314 = FACE_OUTER_BOUND ( 'NONE', #15556, .T. ) ;
#8315 = CARTESIAN_POINT ( 'NONE',  ( 33.61275266354798674, 51.36218137147967866, 93.55433879953098142 ) ) ;
#8316 = VERTEX_POINT ( 'NONE', #451 ) ;
#8317 = EDGE_CURVE ( 'NONE', #899, #18234, #20329, .T. ) ;
#8318 = CARTESIAN_POINT ( 'NONE',  ( 8.945167944750011202, 41.60296030347588214, 76.15680935856015310 ) ) ;
#8319 = EDGE_CURVE ( 'NONE', #8473, #6384, #16840, .T. ) ;
#8320 = EDGE_LOOP ( 'NONE', ( #14393, #12008, #13877, #9232 ) ) ;
#8321 = CARTESIAN_POINT ( 'NONE',  ( 1.256812508749381774, 49.74246873332880625, 95.17996380294498238 ) ) ;
#8322 = CARTESIAN_POINT ( 'NONE',  ( -7.783335128423334304, 41.22810361570975601, 78.64066830726386570 ) ) ;
#8323 = CARTESIAN_POINT ( 'NONE',  ( 5.847829093480187979, 37.15194177590640834, 76.49330797698027595 ) ) ;
#8324 = EDGE_CURVE ( 'NONE', #140, #19954, #13641, .T. ) ;
#8325 = FACE_OUTER_BOUND ( 'NONE', #10975, .T. ) ;
#8326 = ORIENTED_EDGE ( 'NONE', *, *, #19242, .F. ) ;
#8327 = FACE_OUTER_BOUND ( 'NONE', #18590, .T. ) ;
#8328 = ORIENTED_EDGE ( 'NONE', *, *, #1418, .T. ) ;
#8329 = CARTESIAN_POINT ( 'NONE',  ( -7.472485363237701961, 47.84165176951479737, 78.32453815152756249 ) ) ;
#8330 = CARTESIAN_POINT ( 'NONE',  ( -0.9988176903691428077, 49.83852402762217082, 92.05496380123798872 ) ) ;
#8331 = CARTESIAN_POINT ( 'NONE',  ( -3.350035803220276609, 49.20851703305431357, 95.72683880123798872 ) ) ;
#8332 = EDGE_LOOP ( 'NONE', ( #1524, #15135, #13442, #4020, #1668 ) ) ;
#8333 = LINE ( 'NONE', #5228, #19463 ) ;
#8334 = DIRECTION ( 'NONE',  ( 0.3193833840016667702, -0.1065654399787158285, 0.9416146032352017414 ) ) ;
#8335 = CARTESIAN_POINT ( 'NONE',  ( 3.321300766213236333, 39.00526535449171206, 92.55433879953098142 ) ) ;
#8336 = DIRECTION ( 'NONE',  ( -4.142850521348543581E-16, 5.922860397471813007E-17, -1.000000000000000000 ) ) ;
#8337 = DIRECTION ( 'NONE',  ( -3.211742425186504723E-16, 5.922860397471811774E-17, -1.000000000000000000 ) ) ;
#8338 = VERTEX_POINT ( 'NONE', #5652 ) ;
#8339 = LINE ( 'NONE', #14821, #11574 ) ;
#8340 = VERTEX_POINT ( 'NONE', #11955 ) ;
#8341 = CARTESIAN_POINT ( 'NONE',  ( 9.205318032915601023, 42.38264662132202432, 79.33312187154012918 ) ) ;
#8342 = EDGE_CURVE ( 'NONE', #5069, #158, #18431, .T. ) ;
#8343 = CARTESIAN_POINT ( 'NONE',  ( -7.470920617401620945, 40.23538427955658392, 77.87635769503857830 ) ) ;
#8344 = CARTESIAN_POINT ( 'NONE',  ( -4.423078977246956534, 37.62101209537413382, 77.30960331605402303 ) ) ;
#8345 = CARTESIAN_POINT ( 'NONE',  ( 0.7582201636353270713, 49.56899138526064519, 95.21996379611698558 ) ) ;
#8346 = B_SPLINE_CURVE_WITH_KNOTS ( 'NONE', 3,
 ( #8437, #3327, #18012, #14916, #14503, #4911, #1852, #11431, #5018, #17904, #6723, #341, #14610, #38, #16319 ),
 .UNSPECIFIED., .F., .F.,
 ( 4, 1, 1, 1, 1, 1, 1, 1, 1, 1, 1, 1, 4 ),
 ( 0.000000000000000000, 0.1124872259413081665, 0.2145177594606929306, 0.3061691560909166610, 0.3877635431594634863, 0.4596729905988826692, 0.5233009716387192478, 0.5766443983521717387, 0.6225226080321302202, 0.7076769590374641927, 0.7964950891574525960, 0.8912003305064800651, 1.000000000000000000 ),
 .UNSPECIFIED. ) ;
#8347 = CARTESIAN_POINT ( 'NONE',  ( -4.007890887056448470, 40.01116025973682611, 91.39183879782399345 ) ) ;
#8348 = LINE ( 'NONE', #2271, #11968 ) ;
#8349 = ADVANCED_FACE ( 'NONE', ( #15140 ), #5764, .F. ) ;
#8350 = LINE ( 'NONE', #5139, #3037 ) ;
#8351 = EDGE_CURVE ( 'NONE', #14152, #16609, #12158, .T. ) ;
#8352 = EDGE_CURVE ( 'NONE', #12006, #3927, #2778, .T. ) ;
#8353 = EDGE_LOOP ( 'NONE', ( #4950, #12063, #870, #11981 ) ) ;
#8354 = CARTESIAN_POINT ( 'NONE',  ( 27.63948732994508717, 43.16218137147969003, 74.70433879953098710 ) ) ;
#8355 = DIRECTION ( 'NONE',  ( 0.007885122365275663500, 0.9999689119394085113, 1.805443505845543142E-16 ) ) ;
#8356 = ORIENTED_EDGE ( 'NONE', *, *, #2981, .T. ) ;
#8357 = FACE_OUTER_BOUND ( 'NONE', #14761, .T. ) ;
#8358 = PLANE ( 'NONE',  #13658 ) ;
#8359 = CARTESIAN_POINT ( 'NONE',  ( 4.987494971863720927, 47.58855820898865829, 95.96121379953099506 ) ) ;
#8360 = ORIENTED_EDGE ( 'NONE', *, *, #763, .T. ) ;
#8361 = CARTESIAN_POINT ( 'NONE',  ( -0.9988176903691428077, 49.83852402762217082, 95.80496380123798872 ) ) ;
#8362 = CARTESIAN_POINT ( 'NONE',  ( -4.309294135009902327, 37.72656918548430127, 75.36046818803191627 ) ) ;
#8363 = ORIENTED_EDGE ( 'NONE', *, *, #19058, .F. ) ;
#8364 = PLANE ( 'NONE',  #17603 ) ;
#8365 = LINE ( 'NONE', #11674, #17326 ) ;
#8366 = CARTESIAN_POINT ( 'NONE',  ( 1.868012774839550749, 39.13936707477651566, 94.32058879953099506 ) ) ;
#8367 = ORIENTED_EDGE ( 'NONE', *, *, #20772, .F. ) ;
#8368 =( BOUNDED_CURVE ( )  B_SPLINE_CURVE ( 2, ( #8932, #12224, #10858, #20509, #18601, #10754, #15633, #4015, #17219, #10536, #17006 ),
 .UNSPECIFIED., .F., .F. ) 
 B_SPLINE_CURVE_WITH_KNOTS ( ( 3, 2, 2, 2, 2, 3 ),
 ( 0.1389341928972610829, 0.1562449552883616588, 0.1822857811697578267, 0.2083266070511540224, 0.2343674329325501626, 0.2430974982970244558 ),
 .UNSPECIFIED. ) 
 CURVE ( )  GEOMETRIC_REPRESENTATION_ITEM ( )  RATIONAL_B_SPLINE_CURVE ( ( 0.9660722130355270387, 0.9493985585634596713, 1.000000000000000000, 0.9238795325112867385, 1.000000000000000000, 0.9238795325112867385, 1.000000000000000000, 0.9238795325112867385, 1.000000000000000000, 0.9744809684693772622, 0.9660722094251257275 ) ) 
 REPRESENTATION_ITEM ( '' )  );
#8369 = CARTESIAN_POINT ( 'NONE',  ( -4.525688498162991458, 36.95040448855564108, 78.17872471894986575 ) ) ;
#8370 = VERTEX_POINT ( 'NONE', #8757 ) ;
#8371 = LINE ( 'NONE', #11577, #5683 ) ;
#8372 = CARTESIAN_POINT ( 'NONE',  ( 0.5221537403065019678, 44.16218137147968292, 72.45433879953087342 ) ) ;
#8373 = EDGE_CURVE ( 'NONE', #10515, #18997, #15456, .T. ) ;
#8374 = CARTESIAN_POINT ( 'NONE',  ( 6.241727703577843123, 50.87777708829695200, 75.41423045364997790 ) ) ;
#8375 = CARTESIAN_POINT ( 'NONE',  ( -0.1994209430448784792, 35.36759766960258844, 76.86610350541323555 ) ) ;
#8376 = VERTEX_POINT ( 'NONE', #18754 ) ;
#8377 = CARTESIAN_POINT ( 'NONE',  ( 4.753159030984773992, 36.36973062767617648, 75.61597629374708163 ) ) ;
#8378 = CARTESIAN_POINT ( 'NONE',  ( 8.386782761808312614, 39.92944448690413140, 78.16120960217517677 ) ) ;
#8379 = ORIENTED_EDGE ( 'NONE', *, *, #18296, .T. ) ;
#8380 = DIRECTION ( 'NONE',  ( -1.110223024625156540E-16, -1.000000000000000000, -5.922860397471808077E-17 ) ) ;
#8381 = CARTESIAN_POINT ( 'NONE',  ( 8.530801708727521415, 42.72549645772559046, 75.64289537645213102 ) ) ;
#8382 = PLANE ( 'NONE',  #5477 ) ;
#8383 = CARTESIAN_POINT ( 'NONE',  ( 1.851994483447819917, 52.86147903094889244, 79.19202123453014508 ) ) ;
#8384 = ORIENTED_EDGE ( 'NONE', *, *, #16723, .F. ) ;
#8385 = AXIS2_PLACEMENT_3D ( 'NONE', #19068, #20549, #9187 ) ;
#8386 = CARTESIAN_POINT ( 'NONE',  ( 5.393087686338802200, 50.75151780712508298, 78.93669174070734584 ) ) ;
#8387 = ORIENTED_EDGE ( 'NONE', *, *, #17707, .T. ) ;
#8388 = FACE_OUTER_BOUND ( 'NONE', #15026, .T. ) ;
#8389 = B_SPLINE_CURVE_WITH_KNOTS ( 'NONE', 3,
 ( #2336, #11927, #17018, #9046, #7109, #15534, #15328, #17127, #8634, #8832, #7440, #5845, #738, #16709, #7223, #13721, #15114, #2448, #7002 ),
 .UNSPECIFIED., .F., .F.,
 ( 4, 1, 1, 1, 1, 1, 1, 1, 1, 1, 1, 1, 1, 1, 1, 1, 4 ),
 ( 0.000000000000000000, 0.09593561818428578136, 0.1790132514218915338, 0.2495659677033479074, 0.3103928923273128748, 0.3657232523743771391, 0.4198889549570182789, 0.4761292045875803458, 0.5349114402766786958, 0.5687027968553886037, 0.6100175737345402416, 0.6575813992106814831, 0.7121752348458817439, 0.7738275843818921418, 0.8419112148355063496, 0.9177342363179752383, 1.000000000000000000 ),
 .UNSPECIFIED. ) ;
#8390 = EDGE_CURVE ( 'NONE', #7590, #899, #13848, .T. ) ;
#8391 = PLANE ( 'NONE',  #3621 ) ;
#8392 = FACE_OUTER_BOUND ( 'NONE', #4107, .T. ) ;
#8393 = CARTESIAN_POINT ( 'NONE',  ( 8.378259716512932442, 41.81237273359645457, 77.23509376690508077 ) ) ;
#8394 = CARTESIAN_POINT ( 'NONE',  ( 4.419036743624424446, 51.37729090045076674, 79.26137706927028148 ) ) ;
#8395 = CARTESIAN_POINT ( 'NONE',  ( 2.921181103050038974, 49.30691215337508737, 93.34496379782397923 ) ) ;
#8396 = CARTESIAN_POINT ( 'NONE',  ( 6.828503391016846891, 43.33193468930419101, 94.00808880123805977 ) ) ;
#8397 = CARTESIAN_POINT ( 'NONE',  ( 6.477080015414021119, 49.77909886912638626, 76.08942471621537607 ) ) ;
#8398 = CARTESIAN_POINT ( 'NONE',  ( 4.149796636236800396, 51.49816935263167039, 76.01224951307210631 ) ) ;
#8399 = CARTESIAN_POINT ( 'NONE',  ( -3.080359849264385552, 36.80763138399021273, 76.21065298426071877 ) ) ;
#8400 = CARTESIAN_POINT ( 'NONE',  ( 5.568489401881125289, 48.03437091500646261, 91.66433880123796030 ) ) ;
#8401 = VECTOR ( 'NONE', #7981, 1000.000000000000000 ) ;
#8402 = CARTESIAN_POINT ( 'NONE',  ( -0.9988176903691428077, 49.83852402762217082, 93.14871380123798872 ) ) ;
#8403 = VERTEX_POINT ( 'NONE', #8869 ) ;
#8404 = DIRECTION ( 'NONE',  ( 1.000000000000000000, 0.000000000000000000, 0.000000000000000000 ) ) ;
#8405 = DIRECTION ( 'NONE',  ( 0.5813877811927012917, -0.8136266022444372803, -5.636455622144620416E-17 ) ) ;
#8406 = LINE ( 'NONE', #13407, #6539 ) ;
#8407 = EDGE_CURVE ( 'NONE', #18186, #7909, #15247, .T. ) ;
#8408 = CARTESIAN_POINT ( 'NONE',  ( 0.3201111382462866750, 51.36399839264385037, 77.76169174070734869 ) ) ;
#8409 = CARTESIAN_POINT ( 'NONE',  ( 0.5221537403065005245, 44.16218137147968292, 82.45433879953087342 ) ) ;
#8410 = CARTESIAN_POINT ( 'NONE',  ( 8.596205818237969254, 40.55709867257476731, 75.50010622114506020 ) ) ;
#8411 = ORIENTED_EDGE ( 'NONE', *, *, #20011, .T. ) ;
#8412 = ORIENTED_EDGE ( 'NONE', *, *, #13526, .F. ) ;
#8413 = MECHANICAL_DESIGN_GEOMETRIC_PRESENTATION_REPRESENTATION (  '', ( #9444 ), #19937 ) ;
#8414 = CARTESIAN_POINT ( 'NONE',  ( 0.1758192580184792242, 52.20865614724360881, 79.52116152017964623 ) ) ;
#8415 = CARTESIAN_POINT ( 'NONE',  ( 6.326494392126531530, 38.41375405554234845, 78.00072712051441215 ) ) ;
#8416 = DIRECTION ( 'NONE',  ( 1.000000000000000000, 0.000000000000000000, 0.000000000000000000 ) ) ;
#8417 = CARTESIAN_POINT ( 'NONE',  ( 0.8485541085179806320, 52.95612604475941509, 76.28587793549699825 ) ) ;
#8418 = ORIENTED_EDGE ( 'NONE', *, *, #13517, .T. ) ;
#8419 = CARTESIAN_POINT ( 'NONE',  ( -4.414789981656704221, 51.45019435834255717, 78.82303764823565473 ) ) ;
#8420 = LINE ( 'NONE', #10460, #6450 ) ;
#8421 = EDGE_CURVE ( 'NONE', #8103, #2109, #20985, .T. ) ;
#8422 = ORIENTED_EDGE ( 'NONE', *, *, #8730, .F. ) ;
#8423 = CARTESIAN_POINT ( 'NONE',  ( -0.2125050281363792815, 38.58189400963055959, 94.55496380294496817 ) ) ;
#8424 = AXIS2_PLACEMENT_3D ( 'NONE', #10899, #17368, #12582 ) ;
#8425 = DIRECTION ( 'NONE',  ( -1.084202172485505420E-16, -1.000000000000000000, 0.000000000000000000 ) ) ;
#8426 = CARTESIAN_POINT ( 'NONE',  ( 5.568489401881125289, 48.03437091500646261, 95.41433880123797451 ) ) ;
#8427 = DIRECTION ( 'NONE',  ( -0.9534635866061451637, -0.3015081906286224411, -2.009271279954815058E-16 ) ) ;
#8428 = ORIENTED_EDGE ( 'NONE', *, *, #5992, .F. ) ;
#8429 = LINE ( 'NONE', #544, #49 ) ;
#8430 = ORIENTED_EDGE ( 'NONE', *, *, #18862, .T. ) ;
#8431 = CYLINDRICAL_SURFACE ( 'NONE', #14947, 4.999999999999997335 ) ;
#8432 = LINE ( 'NONE', #19389, #9165 ) ;
#8433 = ORIENTED_EDGE ( 'NONE', *, *, #8577, .F. ) ;
#8434 = DIRECTION ( 'NONE',  ( -1.084202172485505420E-16, -1.000000000000000000, 0.000000000000000000 ) ) ;
#8435 = CYLINDRICAL_SURFACE ( 'NONE', #2132, 0.9921021478795020165 ) ;
#8436 = CIRCLE ( 'NONE', #5351, 4.200000000000000178 ) ;
#8437 = CARTESIAN_POINT ( 'NONE',  ( 5.939900590116411472, 51.10072461867315496, 76.38301527011910252 ) ) ;
#8438 = CARTESIAN_POINT ( 'NONE',  ( -1.077846259693493680, 47.82824192744436687, 61.55433879953100273 ) ) ;
#8439 = CARTESIAN_POINT ( 'NONE',  ( 5.076572431691916520, 37.34329067111212197, 72.45433879953087342 ) ) ;
#8440 = ORIENTED_EDGE ( 'NONE', *, *, #8462, .T. ) ;
#8441 = CARTESIAN_POINT ( 'NONE',  ( -4.182948190183843451, 50.86894458203908442, 75.97373057797423712 ) ) ;
#8442 = EDGE_CURVE ( 'NONE', #19492, #2056, #8658, .T. ) ;
#8443 = ORIENTED_EDGE ( 'NONE', *, *, #2589, .T. ) ;
#8444 = DIRECTION ( 'NONE',  ( -0.3165065846431826535, -0.9485903129789529098, -2.188653791613874008E-16 ) ) ;
#8445 = CARTESIAN_POINT ( 'NONE',  ( -7.435799528285976123, 40.12432036608910124, 78.15415281222085753 ) ) ;
#8446 = FACE_OUTER_BOUND ( 'NONE', #15300, .T. ) ;
#8447 = CARTESIAN_POINT ( 'NONE',  ( 4.178421596892070156, 40.17206517740157778, 93.50121379611699979 ) ) ;
#8448 = CARTESIAN_POINT ( 'NONE',  ( 11.22215374030649926, 42.96218137147968008, 77.80433879953099563 ) ) ;
#8449 = CARTESIAN_POINT ( 'NONE',  ( 5.856396280011939126, 46.10368687828906076, 94.43871379782397923 ) ) ;
#8450 = LINE ( 'NONE', #10276, #14672 ) ;
#8451 = B_SPLINE_CURVE_WITH_KNOTS ( 'NONE', 3,
 ( #101, #10984, #14469, #11085, #3088, #6166, #17455, #20933 ),
 .UNSPECIFIED., .F., .F.,
 ( 4, 2, 2, 4 ),
 ( 0.000000000000000000, 0.0001360895826664835205, 0.0002721791653329670409, 0.0005443583306659316966 ),
 .UNSPECIFIED. ) ;
#8452 =( REPRESENTATION_RELATIONSHIP ('NONE','NONE', #11365, #9739 ) REPRESENTATION_RELATIONSHIP_WITH_TRANSFORMATION ( #15499 )SHAPE_REPRESENTATION_RELATIONSHIP( ) );
#8453 = CARTESIAN_POINT ( 'NONE',  ( -7.548577791137153881, 47.77306291863948928, 78.32234914140835258 ) ) ;
#8454 = VECTOR ( 'NONE', #7782, 1000.000000000000000 ) ;
#8455 = CARTESIAN_POINT ( 'NONE',  ( -4.004103039135145536, 51.74365621125981107, 75.44813358671753178 ) ) ;
#8456 = ORIENTED_EDGE ( 'NONE', *, *, #3034, .F. ) ;
#8457 = CARTESIAN_POINT ( 'NONE',  ( 0.6452515144483527143, 52.96578307438453237, 79.54845644658969661 ) ) ;
#8458 = CARTESIAN_POINT ( 'NONE',  ( 5.308031450093095849, 37.52402081283153734, 78.30432351818811298 ) ) ;
#8459 = EDGE_CURVE ( 'NONE', #11174, #14841, #7798, .T. ) ;
#8460 = ORIENTED_EDGE ( 'NONE', *, *, #8351, .F. ) ;
#8461 = CARTESIAN_POINT ( 'NONE',  ( 0.8503282811412331554, 52.95606000782370870, 78.52566232894263010 ) ) ;
#8462 = EDGE_CURVE ( 'NONE', #9068, #15270, #17468, .T. ) ;
#8463 = CARTESIAN_POINT ( 'NONE',  ( -3.981178359372548492, 46.76218137147973408, 93.85183879953099506 ) ) ;
#8464 = VERTEX_POINT ( 'NONE', #19066 ) ;
#8465 = DIRECTION ( 'NONE',  ( 1.000000000000000000, 0.000000000000000000, 1.196361017915039239E-16 ) ) ;
#8466 = DIRECTION ( 'NONE',  ( 1.110223024625156540E-16, 1.000000000000000000, 5.922860397471808077E-17 ) ) ;
#8467 = ORIENTED_EDGE ( 'NONE', *, *, #19236, .F. ) ;
#8468 = CARTESIAN_POINT ( 'NONE',  ( 2.436687528221644250, 49.84925249003584469, 53.23980501161587853 ) ) ;
#8469 = CARTESIAN_POINT ( 'NONE',  ( 0.4729456550870366205, 52.96207995487667120, 75.98649297057549745 ) ) ;
#8470 = EDGE_CURVE ( 'NONE', #7731, #129, #20547, .T. ) ;
#8471 = CARTESIAN_POINT ( 'NONE',  ( 4.987494971863720927, 47.58855820898865829, 92.21121379953100927 ) ) ;
#8472 = EDGE_CURVE ( 'NONE', #8686, #14654, #4476, .T. ) ;
#8473 = VERTEX_POINT ( 'NONE', #1397 ) ;
#8474 = CARTESIAN_POINT ( 'NONE',  ( 31.03948732994507864, 45.16218137147969003, 77.50433879953099847 ) ) ;
#8475 = VECTOR ( 'NONE', #11273, 1000.000000000000000 ) ;
#8476 = ORIENTED_EDGE ( 'NONE', *, *, #15698, .T. ) ;
#8477 = CARTESIAN_POINT ( 'NONE',  ( -4.442047047865082199, 50.68380202455470851, 76.19771883405211099 ) ) ;
#8478 = CARTESIAN_POINT ( 'NONE',  ( 2.080558424246795379, 52.82310755624531140, 76.12927713265780483 ) ) ;
#8479 = EDGE_CURVE ( 'NONE', #20066, #1091, #18285, .T. ) ;
#8480 = CIRCLE ( 'NONE', #13911, 8.199999999999995737 ) ;
#8481 = DIRECTION ( 'NONE',  ( -0.5813877811926999595, 0.8136266022444381685, 5.636455622144657394E-17 ) ) ;
#8482 = CIRCLE ( 'NONE', #21028, 8.199999999999999289 ) ;
#8483 = CARTESIAN_POINT ( 'NONE',  ( -7.203028914707078734, 41.41235317899835877, 78.58228193349691537 ) ) ;
#8484 = ORIENTED_EDGE ( 'NONE', *, *, #7426, .T. ) ;
#8485 = CARTESIAN_POINT ( 'NONE',  ( 0.5221537403065114047, 44.16218137147969713, 45.55433879953100273 ) ) ;
#8486 = AXIS2_PLACEMENT_3D ( 'NONE', #13280, #18373, #11788 ) ;
#8487 = CARTESIAN_POINT ( 'NONE',  ( 7.677770335231880239, 40.16890731605786158, 78.28891658965622469 ) ) ;
#8488 = EDGE_LOOP ( 'NONE', ( #18672, #4494, #5150, #11992 ) ) ;
#8489 = PLANE ( 'NONE',  #20364 ) ;
#8490 = CARTESIAN_POINT ( 'NONE',  ( 8.405938446954575483, 42.35127334101444063, 75.45386443748748206 ) ) ;
#8491 = CARTESIAN_POINT ( 'NONE',  ( 2.522153740306498193, 49.81903562097208038, 123.5543387995310098 ) ) ;
#8492 = DIRECTION ( 'NONE',  ( 1.000000000000000000, 0.000000000000000000, 0.000000000000000000 ) ) ;
#8493 =( BOUNDED_CURVE ( )  B_SPLINE_CURVE ( 3, ( #16741, #5659, #7475, #984 ),
 .UNSPECIFIED., .F., .T. ) 
 B_SPLINE_CURVE_WITH_KNOTS ( ( 4, 4 ),
 ( 4.530614858972014325, 4.536446781922521154 ),
 .UNSPECIFIED. ) 
 CURVE ( )  GEOMETRIC_REPRESENTATION_ITEM ( )  RATIONAL_B_SPLINE_CURVE ( ( 1.000000000000000000, 0.9999971657248998280, 0.9999971657248998280, 1.000000000000000000 ) ) 
 REPRESENTATION_ITEM ( '' )  );
#8494 = ORIENTED_EDGE ( 'NONE', *, *, #20934, .F. ) ;
#8495 = ORIENTED_EDGE ( 'NONE', *, *, #15524, .T. ) ;
#8496 = VECTOR ( 'NONE', #4580, 1000.000000000000000 ) ;
#8497 = EDGE_CURVE ( 'NONE', #5056, #10886, #13963, .T. ) ;
#8498 = PLANE ( 'NONE',  #792 ) ;
#8499 = EDGE_LOOP ( 'NONE', ( #6185, #20253, #5913, #12783 ) ) ;
#8500 = CARTESIAN_POINT ( 'NONE',  ( 5.421579169047436864, 50.73772679352408232, 75.97340973669622599 ) ) ;
#8501 = DIRECTION ( 'NONE',  ( -1.000000000000000000, 0.000000000000000000, 0.000000000000000000 ) ) ;
#8502 = CARTESIAN_POINT ( 'NONE',  ( -7.349889430531795220, 41.86589664987295123, 78.88458194038388172 ) ) ;
#8503 = CARTESIAN_POINT ( 'NONE',  ( 0.1203869048799174335, 52.95380583232233818, 75.39536708303639045 ) ) ;
#8504 = CARTESIAN_POINT ( 'NONE',  ( -3.638881865704250096, 47.35505628976589065, 94.13950776816832899 ) ) ;
#8505 = CARTESIAN_POINT ( 'NONE',  ( 8.788905609664558582, 41.13463217212708400, 76.28640183395299346 ) ) ;
#8506 = VECTOR ( 'NONE', #159, 999.9999999999998863 ) ;
#8507 = CARTESIAN_POINT ( 'NONE',  ( -4.340948238162491535, 40.55733868359232730, 72.45432679953087529 ) ) ;
#8508 = CARTESIAN_POINT ( 'NONE',  ( 6.433553176315260913, 38.47928099333162777, 75.45433879953088763 ) ) ;
#8509 = CARTESIAN_POINT ( 'NONE',  ( -4.524181921268124462, 40.28999182795290324, 92.28933880123798872 ) ) ;
#8510 = AXIS2_PLACEMENT_3D ( 'NONE', #15916, #1338, #7827 ) ;
#8511 = VECTOR ( 'NONE', #13265, 1000.000000000000000 ) ;
#8512 = CARTESIAN_POINT ( 'NONE',  ( 6.828503391016846891, 43.33193468930419101, 92.75808880123800293 ) ) ;
#8513 = ORIENTED_EDGE ( 'NONE', *, *, #8342, .T. ) ;
#8514 = CARTESIAN_POINT ( 'NONE',  ( 0.3366241274589152899, 52.96752759352020945, 76.19791476666895846 ) ) ;
#8515 = DIRECTION ( 'NONE',  ( -1.540237394707284220E-16, -1.793354297423764243E-16, 1.000000000000000000 ) ) ;
#8516 = CARTESIAN_POINT ( 'NONE',  ( -5.528784567355424784, 50.65417461334718752, 79.23104009678212378 ) ) ;
#8517 = DIRECTION ( 'NONE',  ( -4.731737692062791983E-17, 0.7071067811865500152, 0.7071067811865451302 ) ) ;
#8518 = CARTESIAN_POINT ( 'NONE',  ( 5.544968037009670780, 45.50804040601273925, 90.88308879953099506 ) ) ;
#8519 = CARTESIAN_POINT ( 'NONE',  ( 8.933414522996312002, 41.56773455285687646, 77.44430071719698105 ) ) ;
#8520 = CARTESIAN_POINT ( 'NONE',  ( 2.522153740306509295, 49.81903562097208038, 61.15433879953099705 ) ) ;
#8521 = CARTESIAN_POINT ( 'NONE',  ( 5.025485839985549319, 41.56218137147963887, 93.53933880294496817 ) ) ;
#8522 = ORIENTED_EDGE ( 'NONE', *, *, #20293, .F. ) ;
#8523 = EDGE_LOOP ( 'NONE', ( #18982, #5437, #1529, #18520 ) ) ;
#8524 = VECTOR ( 'NONE', #6374, 1000.000000000000000 ) ;
#8525 = CARTESIAN_POINT ( 'NONE',  ( 6.522560395309022319, 49.75102024682771429, 76.63889762306028786 ) ) ;
#8526 = CARTESIAN_POINT ( 'NONE',  ( 5.240387607648463231, 50.87148932128918943, 75.36192990029346106 ) ) ;
#8527 = CARTESIAN_POINT ( 'NONE',  ( -4.315618344801259276, 37.54118080996789786, 78.93496803530179307 ) ) ;
#8528 = ORIENTED_EDGE ( 'NONE', *, *, #5029, .T. ) ;
#8529 = FACE_OUTER_BOUND ( 'NONE', #19630, .T. ) ;
#8530 = DIRECTION ( 'NONE',  ( -1.000000000000000000, 0.000000000000000000, 0.000000000000000000 ) ) ;
#8531 = ORIENTED_EDGE ( 'NONE', *, *, #19087, .F. ) ;
#8532 = CARTESIAN_POINT ( 'NONE',  ( -3.981178359372548492, 46.76218137147973408, 94.16433880294496817 ) ) ;
#8533 = ORIENTED_EDGE ( 'NONE', *, *, #10703, .T. ) ;
#8534 = EDGE_CURVE ( 'NONE', #3734, #16713, #2665, .T. ) ;
#8535 = CARTESIAN_POINT ( 'NONE',  ( 1.926405151277293504, 52.94175334346884654, 77.08393542551461053 ) ) ;
#8536 = CARTESIAN_POINT ( 'NONE',  ( 5.568489401881125289, 48.03437091500646261, 94.16433880123797451 ) ) ;
#8537 = B_SPLINE_SURFACE_WITH_KNOTS ( 'NONE', 3, 1, ( 
 ( #5883, #2682 ),
 ( #20222, #18758 ),
 ( #4172, #20645 ),
 ( #19070, #13967 ),
 ( #1097, #5975 ),
 ( #6075, #10589 ),
 ( #11001, #2897 ),
 ( #9189, #7257 ),
 ( #17472, #9080 ),
 ( #17057, #4480 ),
 ( #7685, #12476 ),
 ( #15787, #12381 ),
 ( #5657, #20449 ),
 ( #20333, #2796 ),
 ( #7585, #18957 ),
 ( #12164, #12580 ),
 ( #4267, #9297 ),
 ( #10697, #17159 ),
 ( #18645, #982 ) ),
 .UNSPECIFIED., .F., .F., .F.,
 ( 4, 1, 1, 1, 1, 1, 1, 1, 1, 1, 1, 1, 1, 1, 1, 1, 4 ),
 ( 2, 2 ),
 ( 0.000000000000000000, 0.1010931020334112918, 0.1936883160783454683, 0.2783829231069467891, 0.3553896825508546242, 0.4249031060497730494, 0.4877225005288854942, 0.5445694316561201509, 0.5961453798982884189, 0.6449762784811632343, 0.6930678288708707058, 0.7409100032456262808, 0.7895445362486890328, 0.8390228595812658785, 0.8900783947972482624, 0.9435774522572311085, 1.000000000000000000 ),
 ( 0.000000000000000000, 1.000000000000000000 ),
 .UNSPECIFIED. ) ;
#8538 = CARTESIAN_POINT ( 'NONE',  ( 31.22215374030650281, 45.56218137147968861, 78.80433879953099563 ) ) ;
#8539 = EDGE_LOOP ( 'NONE', ( #4255, #16282, #12265, #11819, #20336, #11243, #19500, #5552, #632, #1565 ) ) ;
#8540 = PLANE ( 'NONE',  #4504 ) ;
#8541 = EDGE_LOOP ( 'NONE', ( #2359, #17579, #7527, #10235 ) ) ;
#8542 = CARTESIAN_POINT ( 'NONE',  ( 13.13948732994505875, 45.16218137147969003, 78.60433879953099279 ) ) ;
#8543 = AXIS2_PLACEMENT_3D ( 'NONE', #9486, #4567, #10779 ) ;
#8544 = CARTESIAN_POINT ( 'NONE',  ( 4.394343283833276992, 39.11584570990505938, 91.35183880123798872 ) ) ;
#8545 = ORIENTED_EDGE ( 'NONE', *, *, #2339, .F. ) ;
#8546 = CARTESIAN_POINT ( 'NONE',  ( 0.5221537403065071858, 44.16218137147969713, 69.55433879953100984 ) ) ;
#8547 = CARTESIAN_POINT ( 'NONE',  ( -5.953540064417263800, 38.00510092317821886, 78.67637590524894620 ) ) ;
#8548 = CARTESIAN_POINT ( 'NONE',  ( 5.508100443945853186, 47.59510827513957310, 75.45433879953087342 ) ) ;
#8549 = FACE_OUTER_BOUND ( 'NONE', #3775, .T. ) ;
#8550 = LINE ( 'NONE', #8439, #14347 ) ;
#8551 = ORIENTED_EDGE ( 'NONE', *, *, #18068, .F. ) ;
#8552 = DIRECTION ( 'NONE',  ( -1.540237394707284220E-16, -1.793354297423764243E-16, 1.000000000000000000 ) ) ;
#8553 = ORIENTED_EDGE ( 'NONE', *, *, #19759, .F. ) ;
#8554 = FACE_OUTER_BOUND ( 'NONE', #17160, .T. ) ;
#8555 = CARTESIAN_POINT ( 'NONE',  ( -6.823472211661642639, 40.67201601130748401, 77.53559663939034863 ) ) ;
#8556 = ADVANCED_FACE ( 'NONE', ( #2988 ), #1034, .F. ) ;
#8557 = CARTESIAN_POINT ( 'NONE',  ( -4.924280525269182363, 51.08613106951644767, 75.37785507730471579 ) ) ;
#8558 = CARTESIAN_POINT ( 'NONE',  ( 6.701747691083868474, 50.53797885426168079, 79.21482656134288902 ) ) ;
#8559 = ADVANCED_FACE ( 'NONE', ( #16291 ), #18691, .T. ) ;
#8560 = VECTOR ( 'NONE', #8253, 1000.000000000000000 ) ;
#8561 = B_SPLINE_CURVE_WITH_KNOTS ( 'NONE', 3,
 ( #18890, #2716, #18990, #14098, #18673, #15708, #4299, #4093, #2923, #12613, #12506, #20367, #17397, #20673, #10621, #15496, #907, #5803, #19099, #2823, #5914, #1128, #18789, #1016, #11028, #7509 ),
 .UNSPECIFIED., .F., .F.,
 ( 4, 2, 2, 2, 2, 2, 2, 2, 2, 2, 2, 2, 4 ),
 ( 0.000000000000000000, 0.001302007803442155895, 0.001953011705163233518, 0.002604015606884310923, 0.003906023410326472239, 0.004557027312047547477, 0.005208031213768623581, 0.006510039017210761045, 0.007161042918931838884, 0.007812046820652916723, 0.008463050722373993695, 0.009114054624095072402, 0.01041606242753722808 ),
 .UNSPECIFIED. ) ;
#8562 = CARTESIAN_POINT ( 'NONE',  ( 0.7901638384306278740, 50.30062182352762079, 93.57933879782399345 ) ) ;
#8563 = CARTESIAN_POINT ( 'NONE',  ( 5.848951923618479931, 37.15274410921379911, 76.58742703482498371 ) ) ;
#8564 = MECHANICAL_DESIGN_GEOMETRIC_PRESENTATION_REPRESENTATION (  '', ( #7877 ), #15710 ) ;
#8565 = ORIENTED_EDGE ( 'NONE', *, *, #12393, .F. ) ;
#8566 = CARTESIAN_POINT ( 'NONE',  ( 0.8417336166835989175, 52.96423374080004720, 79.54553221853565503 ) ) ;
#8567 = PLANE ( 'NONE',  #5120 ) ;
#8568 = ORIENTED_EDGE ( 'NONE', *, *, #14446, .T. ) ;
#8569 = CYLINDRICAL_SURFACE ( 'NONE', #674, 0.5999999999999894307 ) ;
#8570 = EDGE_CURVE ( 'NONE', #15837, #8173, #4066, .T. ) ;
#8571 = CARTESIAN_POINT ( 'NONE',  ( 6.102441102155617969, 43.42752260303680600, 95.80496379953099506 ) ) ;
#8572 = CARTESIAN_POINT ( 'NONE',  ( -0.2125050281363792815, 38.58189400963055959, 95.49246379953098085 ) ) ;
#8573 = ORIENTED_EDGE ( 'NONE', *, *, #1941, .T. ) ;
#8574 = CARTESIAN_POINT ( 'NONE',  ( 8.804199926738755622, 41.18047021065184055, 77.88643322029270166 ) ) ;
#8575 = CARTESIAN_POINT ( 'NONE',  ( -5.486635640793876334, 38.59622392959819592, 76.24300064276494027 ) ) ;
#8577 = EDGE_CURVE ( 'NONE', #1268, #15169, #7366, .T. ) ;
#8576 = VERTEX_POINT ( 'NONE', #881 ) ;
#8579 = B_SPLINE_CURVE_WITH_KNOTS ( 'NONE', 3,
 ( #9473, #4653, #15959, #9052, #17342, #17643, #17857, #21030, #1592, #16268, #3493, #19450, #13079, #6465, #3185, #192, #11598, #12969 ),
 .UNSPECIFIED., .F., .F.,
 ( 4, 2, 2, 2, 2, 2, 2, 2, 4 ),
 ( 0.000000000000000000, 0.0007105477805655377281, 0.001065821670848306592, 0.001421095561131075456, 0.001598732506272453275, 0.001776369451413830876, 0.001954006396555208695, 0.002131643341696586296, 0.002842191122262097136 ),
 .UNSPECIFIED. ) ;
#8578 = AXIS2_PLACEMENT_3D ( 'NONE', #16363, #9775, #8276 ) ;
#8580 = CARTESIAN_POINT ( 'NONE',  ( 5.605329808110463219, 51.34785857800776654, 78.76051003739772227 ) ) ;
#8581 = CARTESIAN_POINT ( 'NONE',  ( 3.212180877488374886, 51.27651577472676792, 72.45432679953087529 ) ) ;
#8582 = CARTESIAN_POINT ( 'NONE',  ( -4.500660556396669065, 42.81632233694663370, 91.50808879953098085 ) ) ;
#8583 = AXIS2_PLACEMENT_3D ( 'NONE', #2240, #5309, #10240 ) ;
#8584 = ORIENTED_EDGE ( 'NONE', *, *, #8042, .F. ) ;
#8585 = CARTESIAN_POINT ( 'NONE',  ( -2.167873396875370950, 37.04784696823259793, 72.45433879953085921 ) ) ;
#8586 = CARTESIAN_POINT ( 'NONE',  ( 4.613683346302097199, 40.84891852973634485, 90.69696562749766144 ) ) ;
#8587 = ORIENTED_EDGE ( 'NONE', *, *, #2329, .F. ) ;
#8588 = CARTESIAN_POINT ( 'NONE',  ( 2.263811127080453733, 49.90383875825364157, 61.41268141275705972 ) ) ;
#8589 = CARTESIAN_POINT ( 'NONE',  ( 3.357643116058059984, 50.56218137147968861, 96.05433879953096721 ) ) ;
#8590 = EDGE_CURVE ( 'NONE', #4581, #11255, #3341, .T. ) ;
#8591 = EDGE_CURVE ( 'NONE', #972, #2580, #10594, .T. ) ;
#8592 = EDGE_CURVE ( 'NONE', #16784, #8044, #14673, .T. ) ;
#8593 = CARTESIAN_POINT ( 'NONE',  ( 0.000000000000000000, 0.000000000000000000, 0.000000000000000000 ) ) ;
#8594 = CARTESIAN_POINT ( 'NONE',  ( 6.740887235739653427, 50.50906804926147942, 75.70960632971019777 ) ) ;
#8595 = CARTESIAN_POINT ( 'NONE',  ( 5.581367357135656349, 50.61542532950539197, 76.94912097791375061 ) ) ;
#8596 = VECTOR ( 'NONE', #16912, 1000.000000000000000 ) ;
#8597 = DIRECTION ( 'NONE',  ( -0.9539696396349525154, 0.2999031954727373050, -9.315070279690336121E-17 ) ) ;
#8598 = ORIENTED_EDGE ( 'NONE', *, *, #18825, .T. ) ;
#8599 = ORIENTED_EDGE ( 'NONE', *, *, #2583, .F. ) ;
#8600 = EDGE_CURVE ( 'NONE', #19441, #11891, #10484, .T. ) ;
#8601 = CARTESIAN_POINT ( 'NONE',  ( 4.208856430796397596, 36.90056750005005171, 75.71841013695411959 ) ) ;
#8602 = VECTOR ( 'NONE', #13183, 1000.000000000000000 ) ;
#8603 = CARTESIAN_POINT ( 'NONE',  ( 8.414968994577074923, 40.01392041461337357, 78.89537297773202340 ) ) ;
#8604 = ORIENTED_EDGE ( 'NONE', *, *, #13724, .T. ) ;
#8605 = CARTESIAN_POINT ( 'NONE',  ( -4.359893715479207899, 37.57388776543446340, 75.36022115247205022 ) ) ;
#8606 = CARTESIAN_POINT ( 'NONE',  ( 0.5221537403065009686, 44.16218137147968292, 79.45433879953087342 ) ) ;
#8607 = CARTESIAN_POINT ( 'NONE',  ( -0.9988176903691428077, 49.83852402762217082, 93.30496380123798872 ) ) ;
#8608 = ORIENTED_EDGE ( 'NONE', *, *, #15219, .F. ) ;
#8609 = DIRECTION ( 'NONE',  ( 0.000000000000000000, -1.000000000000000000, 3.469446951953617147E-16 ) ) ;
#8610 = VERTEX_POINT ( 'NONE', #13858 ) ;
#8611 = CARTESIAN_POINT ( 'NONE',  ( 0.6452163281857689059, 52.96132085210302165, 79.54845644658969661 ) ) ;
#8612 = AXIS2_PLACEMENT_3D ( 'NONE', #1462, #16350, #6331 ) ;
#8613 = CARTESIAN_POINT ( 'NONE',  ( 25.03948732994508219, 45.16218137147969003, 74.70433879953100131 ) ) ;
#8614 = CARTESIAN_POINT ( 'NONE',  ( 4.546108750497564799, 52.13026250523957827, 76.88467537290178200 ) ) ;
#8615 = CARTESIAN_POINT ( 'NONE',  ( 2.813615989083933844, 36.91585811327295374, 72.45432679953087529 ) ) ;
#8616 = CARTESIAN_POINT ( 'NONE',  ( 2.392664886727887463, 47.70104341108812918, 69.28382765310961133 ) ) ;
#8617 = CARTESIAN_POINT ( 'NONE',  ( 8.798005484913860030, 41.16190507553456968, 76.10950202369875228 ) ) ;
#8618 = B_SPLINE_CURVE_WITH_KNOTS ( 'NONE', 3,
 ( #6095, #14398, #20467, #17694, #3121, #12702, #9316, #20661, #19179, #12491, #6200, #17488, #9624, #17585, #16106, #12399, #4593, #10812, #2914, #17278, #3013, #14182, #9210, #15696, #18978, #7604, #14087 ),
 .UNSPECIFIED., .F., .F.,
 ( 4, 1, 1, 1, 1, 1, 1, 1, 1, 1, 1, 1, 1, 1, 1, 1, 1, 1, 1, 1, 1, 1, 1, 1, 4 ),
 ( 0.000000000000000000, 0.05111620615384394190, 0.09904209687041264087, 0.1432334450931441461, 0.1843589373079111415, 0.2222937343119009146, 0.2574440974212286459, 0.2893637488079585096, 0.3188910630028964910, 0.3474602836591745292, 0.3767670824238625316, 0.4074295047838343287, 0.4392621747742110894, 0.4730325979957886173, 0.5084852716492808122, 0.5462542205972961140, 0.5860610780164621225, 0.6283505634423164343, 0.6729648726644925638, 0.7201947540188263774, 0.7701882088044430530, 0.8230700400259792771, 0.8789456997408242600, 0.9378877171948971636, 1.000000000000000000 ),
 .UNSPECIFIED. ) ;
#8619 = CARTESIAN_POINT ( 'NONE',  ( 8.527988662190095326, 48.03182059810101379, 79.44551527011911674 ) ) ;
#8620 = CARTESIAN_POINT ( 'NONE',  ( 4.544296722651392173, 52.13160097721661401, 76.36737811492949390 ) ) ;
#8621 = EDGE_CURVE ( 'NONE', #17446, #3176, #20227, .T. ) ;
#8622 = CARTESIAN_POINT ( 'NONE',  ( -0.9988176903691428077, 49.83852402762217082, 90.64871380123798872 ) ) ;
#8623 = LINE ( 'NONE', #18605, #16726 ) ;
#8624 = EDGE_LOOP ( 'NONE', ( #15986, #10185, #3715, #6686 ) ) ;
#8625 = EDGE_CURVE ( 'NONE', #16609, #799, #20839, .T. ) ;
#8626 = DIRECTION ( 'NONE',  ( -1.540237394707284220E-16, -1.793354297423764243E-16, 1.000000000000000000 ) ) ;
#8627 =( BOUNDED_CURVE ( )  B_SPLINE_CURVE ( 3, ( #8588, #13370, #5586, #3985 ),
 .UNSPECIFIED., .F., .F. ) 
 B_SPLINE_CURVE_WITH_KNOTS ( ( 4, 4 ),
 ( 5.006904465492826084, 5.052225889838810602 ),
 .UNSPECIFIED. ) 
 CURVE ( )  GEOMETRIC_REPRESENTATION_ITEM ( )  RATIONAL_B_SPLINE_CURVE ( ( 1.000000000000000000, 0.9998288380325438540, 0.9998288380325438540, 1.000000000000000000 ) ) 
 REPRESENTATION_ITEM ( '' )  );
#8628 = ADVANCED_FACE ( 'NONE', ( #563 ), #13545, .F. ) ;
#8629 = AXIS2_PLACEMENT_3D ( 'NONE', #9590, #9379, #12671 ) ;
#8630 = DIRECTION ( 'NONE',  ( 0.007885122365275663500, 0.9999689119394085113, 1.805443505845543142E-16 ) ) ;
#8631 = FACE_OUTER_BOUND ( 'NONE', #9849, .T. ) ;
#8632 = CARTESIAN_POINT ( 'NONE',  ( -4.361349971946749449, 37.58365018120226608, 78.93613021445058564 ) ) ;
#8633 = CARTESIAN_POINT ( 'NONE',  ( -5.784195910403845176, 44.99242805365518194, 92.28933880123798872 ) ) ;
#8634 = CARTESIAN_POINT ( 'NONE',  ( -4.686954935604242145, 37.06952550968519233, 77.27854074750605662 ) ) ;
#8635 = CARTESIAN_POINT ( 'NONE',  ( 0.5221537403065005245, 44.16218137147968292, 82.45433879953087342 ) ) ;
#8636 = ADVANCED_FACE ( 'NONE', ( #5455 ), #16953, .F. ) ;
#8637 = CARTESIAN_POINT ( 'NONE',  ( 9.125273767571993488, 43.16218137147969713, 95.45352954694192249 ) ) ;
#8638 = VERTEX_POINT ( 'NONE', #16537 ) ;
#8639 = CARTESIAN_POINT ( 'NONE',  ( 8.281036760714160394, 41.97693506373668271, 79.53018343098241871 ) ) ;
#8640 = DIRECTION ( 'NONE',  ( -1.779391786395883536E-16, -5.922860397471806844E-17, 1.000000000000000000 ) ) ;
#8641 = CARTESIAN_POINT ( 'NONE',  ( 5.499753608866646104, 50.67865541357578252, 77.99542992962396681 ) ) ;
#8642 = ORIENTED_EDGE ( 'NONE', *, *, #16004, .T. ) ;
#8643 = PLANE ( 'NONE',  #16091 ) ;
#8644 = FACE_OUTER_BOUND ( 'NONE', #16427, .T. ) ;
#8645 = VECTOR ( 'NONE', #14387, 1000.000000000000000 ) ;
#8646 = DIRECTION ( 'NONE',  ( -1.540237394707284220E-16, -1.793354297423764243E-16, 1.000000000000000000 ) ) ;
#8647 = CARTESIAN_POINT ( 'NONE',  ( -2.077846259693550746, 39.65884927180063357, 93.22683880294496817 ) ) ;
#8648 = CARTESIAN_POINT ( 'NONE',  ( 1.706499989092010949, 52.94348737648915204, 76.92027168626151479 ) ) ;
#8649 = CARTESIAN_POINT ( 'NONE',  ( 5.611423337425062385, 41.22389019960463230, 95.17996380123798872 ) ) ;
#8650 = DIRECTION ( 'NONE',  ( -0.000000000000000000, 1.000000000000000000, 1.734723475976787531E-14 ) ) ;
#8651 = ORIENTED_EDGE ( 'NONE', *, *, #16909, .T. ) ;
#8652 = CARTESIAN_POINT ( 'NONE',  ( 27.03948732994508219, 45.16218137147969003, 78.60433879953099279 ) ) ;
#8653 = ORIENTED_EDGE ( 'NONE', *, *, #13000, .T. ) ;
#8654 = CARTESIAN_POINT ( 'NONE',  ( -1.856544280600658459, 49.13739387491266086, 92.96485748750068012 ) ) ;
#8655 = CARTESIAN_POINT ( 'NONE',  ( 6.828503391016846891, 43.33193468930419101, 92.75808880123800293 ) ) ;
#8656 = ORIENTED_EDGE ( 'NONE', *, *, #12708, .F. ) ;
#8657 = CARTESIAN_POINT ( 'NONE',  ( -4.592862224480082745, 51.32295045326189609, 75.97198585835440099 ) ) ;
#8658 = LINE ( 'NONE', #18321, #9483 ) ;
#8659 = LINE ( 'NONE', #20445, #5743 ) ;
#8660 = DIRECTION ( 'NONE',  ( 1.540237394707284467E-16, 1.793354297423764243E-16, -1.000000000000000000 ) ) ;
#8661 = CARTESIAN_POINT ( 'NONE',  ( 5.562547263452509938, 51.37946032036057886, 77.00567114208729436 ) ) ;
#8662 = LINE ( 'NONE', #556, #12666 ) ;
#8663 = ORIENTED_EDGE ( 'NONE', *, *, #15753, .F. ) ;
#8664 = LINE ( 'NONE', #10267, #14957 ) ;
#8665 = ORIENTED_EDGE ( 'NONE', *, *, #15289, .T. ) ;
#8666 = ADVANCED_FACE ( 'NONE', ( #244 ), #1957, .T. ) ;
#8667 = DIRECTION ( 'NONE',  ( 1.540237394707283727E-16, 1.793354297423763257E-16, -1.000000000000000000 ) ) ;
#8668 = CARTESIAN_POINT ( 'NONE',  ( -7.885128509680407127, 41.54523971581953390, 76.16022115247204738 ) ) ;
#8669 = CARTESIAN_POINT ( 'NONE',  ( 6.198496396448986090, 45.68315280215533392, 92.99246380123798872 ) ) ;
#8670 = CARTESIAN_POINT ( 'NONE',  ( 7.691771551572206711, 40.18266124458227750, 72.45433879953087342 ) ) ;
#8671 = CARTESIAN_POINT ( 'NONE',  ( -4.007890887056451135, 40.01116025973682611, 92.79808879782397923 ) ) ;
#8672 = CARTESIAN_POINT ( 'NONE',  ( -3.154801521863568325, 47.83913663364971569, 95.05433879953098142 ) ) ;
#8673 = EDGE_LOOP ( 'NONE', ( #4907, #10181, #8784, #15703 ) ) ;
#8674 = CARTESIAN_POINT ( 'NONE',  ( 8.274641112204461635, 41.51360698326416809, 78.93505401271374922 ) ) ;
#8675 = VERTEX_POINT ( 'NONE', #8448 ) ;
#8676 = LINE ( 'NONE', #1869, #7116 ) ;
#8677 = B_SPLINE_CURVE_WITH_KNOTS ( 'NONE', 3,
 ( #16392, #3399, #17551, #16283, #2978, #7986, #8087, #14576, #9911, #14471, #7773, #14250, #6370, #20733, #12673 ),
 .UNSPECIFIED., .F., .F.,
 ( 4, 1, 1, 1, 1, 1, 1, 1, 1, 1, 1, 1, 4 ),
 ( 0.000000000000000000, 0.07527217715292475186, 0.1459465445934834404, 0.2117756949130734923, 0.2766029815265222958, 0.3381147468631120478, 0.3951637252042238257, 0.4534551218168583753, 0.5124046679576552688, 0.5890284689491043224, 0.6947781202056673155, 0.8321371544603952675, 0.9999999999999998890 ),
 .UNSPECIFIED. ) ;
#8678 = ADVANCED_FACE ( 'NONE', ( #352 ), #20457, .F. ) ;
#8679 = CARTESIAN_POINT ( 'NONE',  ( -3.981178359372548492, 46.76218137147973408, 92.60183879953099506 ) ) ;
#8680 = CARTESIAN_POINT ( 'NONE',  ( 1.868012774839550749, 39.13936707477651566, 91.82058879953099506 ) ) ;
#8681 = ORIENTED_EDGE ( 'NONE', *, *, #13097, .F. ) ;
#8682 = FILL_AREA_STYLE ('',( #10395 ) ) ;
#8683 = CARTESIAN_POINT ( 'NONE',  ( -2.416137431568557314, 39.07291177436112406, 94.86746380123805977 ) ) ;
#8684 = CARTESIAN_POINT ( 'NONE',  ( 3.722852957781953798, 40.32059543431686421, 95.05433879953096721 ) ) ;
#8685 = CARTESIAN_POINT ( 'NONE',  ( 13.32277635493561974, 51.36218137147968577, 80.55433879953099563 ) ) ;
#8686 = VERTEX_POINT ( 'NONE', #9089 ) ;
#8687 = CARTESIAN_POINT ( 'NONE',  ( -1.677846259693499542, 50.36218137147968577, 50.15433879953098995 ) ) ;
#8688 = ORIENTED_EDGE ( 'NONE', *, *, #11507, .F. ) ;
#8689 = CARTESIAN_POINT ( 'NONE',  ( -4.774380534136511756, 51.19324411499089678, 76.08363728426196815 ) ) ;
#8690 = DIRECTION ( 'NONE',  ( -0.9999689119394086223, 0.007885122365275665235, -1.526048693634353392E-16 ) ) ;
#8691 = CARTESIAN_POINT ( 'NONE',  ( -4.524181921268124462, 40.28999182795290324, 91.03933880123798872 ) ) ;
#8692 = CARTESIAN_POINT ( 'NONE',  ( 0.000000000000000000, 0.000000000000000000, 0.000000000000000000 ) ) ;
#8693 = CARTESIAN_POINT ( 'NONE',  ( -3.545047478496393456, 36.22604446995779881, 78.23707788297487298 ) ) ;
#8694 = EDGE_CURVE ( 'NONE', #13124, #12799, #4072, .T. ) ;
#8695 = DIRECTION ( 'NONE',  ( 1.193617070626243484E-16, 1.000000000000000000, 0.000000000000000000 ) ) ;
#8696 = CARTESIAN_POINT ( 'NONE',  ( -3.098709854545130593, 36.80491647020841128, 78.46683879953087626 ) ) ;
#8697 = ORIENTED_EDGE ( 'NONE', *, *, #17069, .T. ) ;
#8698 = EDGE_LOOP ( 'NONE', ( #9489, #14853, #17466, #9601, #581, #18904 ) ) ;
#8699 = CARTESIAN_POINT ( 'NONE',  ( -0.4699484075730043786, 51.36218137147968577, 52.53721119516358584 ) ) ;
#8700 = EDGE_CURVE ( 'NONE', #11467, #15461, #14078, .T. ) ;
#8701 = ORIENTED_EDGE ( 'NONE', *, *, #20704, .F. ) ;
#8702 = CARTESIAN_POINT ( 'NONE',  ( 2.522153740306506631, 50.16218137147969713, 77.15433879953100416 ) ) ;
#8703 = CARTESIAN_POINT ( 'NONE',  ( 0.4250111554052659057, 52.35549180149831727, 77.42486900944150818 ) ) ;
#8704 = CARTESIAN_POINT ( 'NONE',  ( 6.828503391016846891, 43.33193468930419101, 94.16433880123797451 ) ) ;
#8705 = EDGE_LOOP ( 'NONE', ( #103, #17370, #17586, #1420 ) ) ;
#8706 = CARTESIAN_POINT ( 'NONE',  ( 6.885459498894642927, 50.40227834219487590, 78.84682786933051091 ) ) ;
#8707 = ORIENTED_EDGE ( 'NONE', *, *, #768, .F. ) ;
#8708 = CARTESIAN_POINT ( 'NONE',  ( 10.77494014480653561, 42.96218137147968008, 66.20574467885104752 ) ) ;
#8709 = CARTESIAN_POINT ( 'NONE',  ( 6.882377701754223587, 37.89119233413698140, 76.59354538285809610 ) ) ;
#8710 = CARTESIAN_POINT ( 'NONE',  ( 11.22215374030650281, 45.56218137147968150, 56.80715055817104542 ) ) ;
#8711 = CARTESIAN_POINT ( 'NONE',  ( -3.552306130656605720, 51.28101034580461004, 79.43132126585329900 ) ) ;
#8712 = CARTESIAN_POINT ( 'NONE',  ( -0.5476599173704348456, 52.89753068181172324, 75.65267637979816584 ) ) ;
#8713 = FACE_OUTER_BOUND ( 'NONE', #7170, .T. ) ;
#8714 = PRODUCT_DEFINITION_SHAPE ( 'NONE', 'NONE',  #21039 ) ;
#8715 = CARTESIAN_POINT ( 'NONE',  ( 8.868817592801745420, 41.37413345511091478, 75.97198585835440099 ) ) ;
#8716 = LINE ( 'NONE', #7209, #19685 ) ;
#8717 = CARTESIAN_POINT ( 'NONE',  ( -1.219056181852248066, 49.77488197367201650, 94.48425466814985896 ) ) ;
#8718 = CARTESIAN_POINT ( 'NONE',  ( -5.154188915835984375, 42.64120994080404614, 90.96121380123797451 ) ) ;
#8719 = CARTESIAN_POINT ( 'NONE',  ( 8.346529106983265223, 41.70870148392067023, 76.02106044755406344 ) ) ;
#8720 = DIRECTION ( 'NONE',  ( -0.000000000000000000, -0.000000000000000000, 1.000000000000000000 ) ) ;
#8721 = ORIENTED_EDGE ( 'NONE', *, *, #9073, .T. ) ;
#8722 = LINE ( 'NONE', #7103, #17329 ) ;
#8723 = CARTESIAN_POINT ( 'NONE',  ( 8.214799251806553571, 41.32260305165857517, 78.45948585835439815 ) ) ;
#8724 = DIRECTION ( 'NONE',  ( 1.193617070626243484E-16, 1.000000000000000000, 0.000000000000000000 ) ) ;
#8725 = CARTESIAN_POINT ( 'NONE',  ( 2.043125170982144745, 38.48583871533720213, 95.17996380123798872 ) ) ;
#8726 = EDGE_CURVE ( 'NONE', #2422, #13701, #12388, .T. ) ;
#8727 = CARTESIAN_POINT ( 'NONE',  ( -5.677846259693490438, 44.16218137147969003, 111.0905869729573681 ) ) ;
#8728 = DIRECTION ( 'NONE',  ( 1.540237394707284220E-16, 1.793354297423764243E-16, -1.000000000000000000 ) ) ;
#8729 = CARTESIAN_POINT ( 'NONE',  ( 3.547567743947614538, 48.49067789217866675, 94.73725702289965511 ) ) ;
#8730 = EDGE_CURVE ( 'NONE', #15997, #18224, #4276, .T. ) ;
#8731 = CARTESIAN_POINT ( 'NONE',  ( 5.761154613439540384, 51.23275707131721646, 77.94923276678728996 ) ) ;
#8732 = ORIENTED_EDGE ( 'NONE', *, *, #12606, .F. ) ;
#8733 = ORIENTED_EDGE ( 'NONE', *, *, #4789, .F. ) ;
#8734 = CARTESIAN_POINT ( 'NONE',  ( 6.507769556168451430, 49.76686128376767471, 77.01032402965913093 ) ) ;
#8735 = CARTESIAN_POINT ( 'NONE',  ( -4.680892486399498509, 37.06504742266799468, 75.36060488990274564 ) ) ;
#8736 = ADVANCED_FACE ( 'NONE', ( #991 ), #5985, .T. ) ;
#8737 = CARTESIAN_POINT ( 'NONE',  ( -7.677846259693483333, 47.36218137147966445, 93.55433879953098142 ) ) ;
#8738 = ORIENTED_EDGE ( 'NONE', *, *, #13380, .F. ) ;
#8739 = CARTESIAN_POINT ( 'NONE',  ( 0.5351667827239598996, 52.36231569124743146, 78.93477473415802592 ) ) ;
#8740 = DIRECTION ( 'NONE',  ( -0.5941461771851693774, -0.8043570849667760481, -2.357623395011396791E-16 ) ) ;
#8741 = EDGE_CURVE ( 'NONE', #15118, #2200, #15471, .T. ) ;
#8742 = AXIS2_PLACEMENT_3D ( 'NONE', #13343, #13443, #15042 ) ;
#8743 = CARTESIAN_POINT ( 'NONE',  ( -2.313335635445063598, 50.56218137147968861, 92.03489701350649455 ) ) ;
#8744 = CARTESIAN_POINT ( 'NONE',  ( 1.868012774839550749, 39.13936707477651566, 93.38308880294498238 ) ) ;
#8745 =( BOUNDED_CURVE ( )  B_SPLINE_CURVE ( 3, ( #14625, #1764, #14730, #11134 ),
 .UNSPECIFIED., .F., .F. ) 
 B_SPLINE_CURVE_WITH_KNOTS ( ( 4, 4 ),
 ( 1.415673517910795987, 1.520829339303995331 ),
 .UNSPECIFIED. ) 
 CURVE ( )  GEOMETRIC_REPRESENTATION_ITEM ( )  RATIONAL_B_SPLINE_CURVE ( ( 1.000000000000000000, 0.9990787333635395839, 0.9990787333635395839, 1.000000000000000000 ) ) 
 REPRESENTATION_ITEM ( '' )  );
#8746 = CARTESIAN_POINT ( 'NONE',  ( -7.783107710516365962, 41.22738444886793729, 78.61536821129558916 ) ) ;
#8747 = CARTESIAN_POINT ( 'NONE',  ( -4.567115856812060670, 47.10047254335474065, 93.30496380123798872 ) ) ;
#8748 = LINE ( 'NONE', #15132, #16022 ) ;
#8749 = VERTEX_POINT ( 'NONE', #12484 ) ;
#8750 = LINE ( 'NONE', #15238, #4460 ) ;
#8751 = ORIENTED_EDGE ( 'NONE', *, *, #14814, .T. ) ;
#8752 = AXIS2_PLACEMENT_3D ( 'NONE', #1378, #12553, #17232 ) ;
#8753 = CARTESIAN_POINT ( 'NONE',  ( -4.265367546595294712, 50.81005072751269580, 78.93596273702843291 ) ) ;
#8754 = CARTESIAN_POINT ( 'NONE',  ( 1.352400422481993658, 50.46853102219002096, 90.57058880123798872 ) ) ;
#8755 = VERTEX_POINT ( 'NONE', #15369 ) ;
#8756 = DIRECTION ( 'NONE',  ( 0.6080936526121289987, 0.7938652969193448206, 2.360290325043240801E-16 ) ) ;
#8757 = CARTESIAN_POINT ( 'NONE',  ( -4.158578283022522193, 37.42937009194850617, 76.81463291717793140 ) ) ;
#8758 = CARTESIAN_POINT ( 'NONE',  ( -3.343753456003188518, 51.29574226414619886, 79.34012906335151172 ) ) ;
#8759 = LINE ( 'NONE', #10477, #5344 ) ;
#8760 = DIRECTION ( 'NONE',  ( 1.540237394707284220E-16, 1.793354297423764243E-16, -1.000000000000000000 ) ) ;
#8761 = ADVANCED_FACE ( 'NONE', ( #18966 ), #15685, .F. ) ;
#8762 = CARTESIAN_POINT ( 'NONE',  ( -1.477846259693489817, 49.16218137147969003, 50.55433879953100273 ) ) ;
#8763 = VERTEX_POINT ( 'NONE', #5782 ) ;
#8764 = CARTESIAN_POINT ( 'NONE',  ( 5.241898597225179479, 50.86770213969851540, 78.23114816710980790 ) ) ;
#8765 = VECTOR ( 'NONE', #3416, 1000.000000000000000 ) ;
#8766 = VERTEX_POINT ( 'NONE', #4379 ) ;
#8767 = CARTESIAN_POINT ( 'NONE',  ( 1.514255888186003984, 52.36218137147968577, 83.03825919817350609 ) ) ;
#8768 = DIRECTION ( 'NONE',  ( 6.308085367188358095E-15, 8.847205979147994320E-31, 1.000000000000000000 ) ) ;
#8769 = CARTESIAN_POINT ( 'NONE',  ( 10.77494014480653917, 42.76218137147968434, 61.40715055817103263 ) ) ;
#8770 = DIRECTION ( 'NONE',  ( -1.540237394707284220E-16, -1.793354297423764243E-16, 1.000000000000000000 ) ) ;
#8771 = CARTESIAN_POINT ( 'NONE',  ( -3.628867371436363509, 48.69222599884265179, 92.48558879782397923 ) ) ;
#8772 = CARTESIAN_POINT ( 'NONE',  ( 1.652727357819364640, 35.35299279957455809, 75.45433879953087342 ) ) ;
#8773 = ORIENTED_EDGE ( 'NONE', *, *, #20113, .T. ) ;
#8774 = CARTESIAN_POINT ( 'NONE',  ( 4.103056440471904764, 51.53898521715114356, 76.82013224188756340 ) ) ;
#8775 = AXIS2_PLACEMENT_3D ( 'NONE', #10461, #16926, #9589 ) ;
#8776 = VERTEX_POINT ( 'NONE', #17374 ) ;
#8777 = CARTESIAN_POINT ( 'NONE',  ( -4.387981331227590154, 51.46935083841186298, 75.37146543928014353 ) ) ;
#8778 = CARTESIAN_POINT ( 'NONE',  ( 6.102441102155617969, 43.42752260303680600, 92.05496379953099506 ) ) ;
#8779 = CARTESIAN_POINT ( 'NONE',  ( 3.122153740306552905, 48.66551347115873227, 92.28933879953099506 ) ) ;
#8780 = ORIENTED_EDGE ( 'NONE', *, *, #2197, .T. ) ;
#8781 = B_SPLINE_CURVE_WITH_KNOTS ( 'NONE', 3,
 ( #2722, #4514, #9227, #11033, #15715, #1133, #7621, #14103, #4410, #17503, #20585, #2927, #6013, #9429, #7721 ),
 .UNSPECIFIED., .F., .F.,
 ( 4, 1, 1, 1, 1, 1, 1, 1, 1, 1, 1, 1, 4 ),
 ( 0.000000000000000000, 0.1107947361882193060, 0.2116365373969002206, 0.3025951166517907298, 0.3827141919669941328, 0.4557983700405009997, 0.5187458605491411801, 0.5729830782426720281, 0.6198356358567430613, 0.7053145269299332387, 0.7944869293383459707, 0.8901174066118697770, 1.000000000000000000 ),
 .UNSPECIFIED. ) ;
#8782 = CARTESIAN_POINT ( 'NONE',  ( -4.409036544953043979, 47.67330854490502645, 75.45433879953087342 ) ) ;
#8783 = LINE ( 'NONE', #1006, #15040 ) ;
#8784 = ORIENTED_EDGE ( 'NONE', *, *, #20820, .T. ) ;
#8785 = DIRECTION ( 'NONE',  ( -0.000000000000000000, -0.000000000000000000, 1.000000000000000000 ) ) ;
#8786 = DIRECTION ( 'NONE',  ( -1.402518428993831183E-16, 1.000000000000000000, -3.469446951953617640E-16 ) ) ;
#8787 = ORIENTED_EDGE ( 'NONE', *, *, #16781, .F. ) ;
#8788 = LINE ( 'NONE', #7505, #9872 ) ;
#8789 = CARTESIAN_POINT ( 'NONE',  ( -5.784195910403845176, 44.99242805365518194, 93.53933880123797451 ) ) ;
#8790 = EDGE_LOOP ( 'NONE', ( #12887, #4667, #2421, #16916 ) ) ;
#8791 = CARTESIAN_POINT ( 'NONE',  ( -4.762271096064603526, 51.20189707608225405, 76.05031124229590489 ) ) ;
#8792 = PLANE ( 'NONE',  #15649 ) ;
#8793 = VECTOR ( 'NONE', #18953, 1000.000000000000000 ) ;
#8794 = LINE ( 'NONE', #2408, #17458 ) ;
#8795 = DIRECTION ( 'NONE',  ( -0.000000000000000000, -0.000000000000000000, 1.000000000000000000 ) ) ;
#8796 = EDGE_CURVE ( 'NONE', #9334, #10505, #7267, .T. ) ;
#8797 = DIRECTION ( 'NONE',  ( -0.5813877811927011807, 0.8136266022444372803, 5.636455622144619183E-17 ) ) ;
#8798 = ORIENTED_EDGE ( 'NONE', *, *, #6845, .T. ) ;
#8799 = ORIENTED_EDGE ( 'NONE', *, *, #3605, .F. ) ;
#8800 = CARTESIAN_POINT ( 'NONE',  ( 1.972616468458138650, 52.95547850198470030, 75.87378281519762879 ) ) ;
#8801 = VERTEX_POINT ( 'NONE', #7692 ) ;
#8802 = CARTESIAN_POINT ( 'NONE',  ( 6.876224750190004897, 50.40909967906462441, 75.93520998463665705 ) ) ;
#8803 = PLANE ( 'NONE',  #12960 ) ;
#8804 = CARTESIAN_POINT ( 'NONE',  ( 6.198496396448986090, 45.68315280215533392, 95.49246380123798872 ) ) ;
#8805 = EDGE_LOOP ( 'NONE', ( #15479, #14486, #10, #5374 ) ) ;
#8806 = AXIS2_PLACEMENT_3D ( 'NONE', #14611, #16320, #9731 ) ;
#8807 = EDGE_CURVE ( 'NONE', #6493, #7731, #9306, .T. ) ;
#8808 = LINE ( 'NONE', #15302, #8272 ) ;
#8809 = VERTEX_POINT ( 'NONE', #6082 ) ;
#8810 = CARTESIAN_POINT ( 'NONE',  ( -3.579922675594000125, 36.25180537319517526, 77.38751485876633751 ) ) ;
#8811 = CARTESIAN_POINT ( 'NONE',  ( -0.1709386726045580007, 50.28109722957945138, 51.67325465763072856 ) ) ;
#8812 = CARTESIAN_POINT ( 'NONE',  ( -4.804644443005472887, 51.17161863374555963, 76.44036821129557779 ) ) ;
#8813 = DIRECTION ( 'NONE',  ( -1.540237394707283727E-16, -1.793354297423763257E-16, 1.000000000000000000 ) ) ;
#8814 = CARTESIAN_POINT ( 'NONE',  ( -7.578484755904182357, 42.88833611937010915, 79.14296897072306081 ) ) ;
#8815 = CARTESIAN_POINT ( 'NONE',  ( 3.460444912181559474, 49.25145096859824889, 94.39871380123798872 ) ) ;
#8816 = CARTESIAN_POINT ( 'NONE',  ( 0.5915713968613123264, 52.96553219837200999, 77.38375056423674891 ) ) ;
#8817 = PLANE ( 'NONE',  #3055 ) ;
#8818 = CARTESIAN_POINT ( 'NONE',  ( 4.566945366853153665, 51.19003838910122539, 75.50506468444432073 ) ) ;
#8819 = CARTESIAN_POINT ( 'NONE',  ( 3.122153740306552905, 48.66551347115873227, 92.60183880294498238 ) ) ;
#8820 = AXIS2_PLACEMENT_3D ( 'NONE', #2017, #8515, #11810 ) ;
#8821 = EDGE_CURVE ( 'NONE', #10817, #7197, #10599, .T. ) ;
#8822 = CARTESIAN_POINT ( 'NONE',  ( 2.722153740306518799, 49.95873206995546667, 54.55433879953099563 ) ) ;
#8823 = VERTEX_POINT ( 'NONE', #4487 ) ;
#8824 = PRESENTATION_STYLE_ASSIGNMENT (( #4446 ) ) ;
#8825 = AXIS2_PLACEMENT_3D ( 'NONE', #13450, #13352, #3656 ) ;
#8826 = EDGE_LOOP ( 'NONE', ( #12983, #11592, #2797, #12368 ) ) ;
#8827 = LINE ( 'NONE', #5401, #2358 ) ;
#8828 = LINE ( 'NONE', #20297, #12636 ) ;
#8829 = CARTESIAN_POINT ( 'NONE',  ( -3.350758615681482144, 52.21051221579373447, 78.23748737924660190 ) ) ;
#8830 = CARTESIAN_POINT ( 'NONE',  ( 3.122153740306552905, 48.66551347115873227, 91.03933879953099506 ) ) ;
#8831 = VECTOR ( 'NONE', #20042, 1000.000000000000000 ) ;
#8832 = CARTESIAN_POINT ( 'NONE',  ( -4.730130202819497143, 37.10141734037124905, 77.29630340639747033 ) ) ;
#8833 = CARTESIAN_POINT ( 'NONE',  ( -6.859224089373359590, 47.65557686534583581, 78.82648837639791850 ) ) ;
#8834 = CARTESIAN_POINT ( 'NONE',  ( -3.621797592085240769, 36.28273668718272660, 77.97675128563095370 ) ) ;
#8835 = ADVANCED_FACE ( 'NONE', ( #17480 ), #7484, .F. ) ;
#8836 = LINE ( 'NONE', #10345, #14922 ) ;
#8837 = VECTOR ( 'NONE', #17841, 1000.000000000000114 ) ;
#8838 = ORIENTED_EDGE ( 'NONE', *, *, #15208, .T. ) ;
#8839 = ORIENTED_EDGE ( 'NONE', *, *, #4123, .T. ) ;
#8840 = AXIS2_PLACEMENT_3D ( 'NONE', #18660, #5899, #10810 ) ;
#8841 = EDGE_CURVE ( 'NONE', #15205, #19372, #965, .T. ) ;
#8842 = CARTESIAN_POINT ( 'NONE',  ( 6.490071791215038743, 49.78570669403264048, 77.16764180776988269 ) ) ;
#8843 = DIRECTION ( 'NONE',  ( -0.000000000000000000, -0.000000000000000000, 1.000000000000000000 ) ) ;
#8844 = LINE ( 'NONE', #18834, #3139 ) ;
#8845 = LINE ( 'NONE', #12357, #4515 ) ;
#8846 = CARTESIAN_POINT ( 'NONE',  ( -1.998366399307998753, 38.86341998953714238, 95.05433879953095300 ) ) ;
#8847 = AXIS2_PLACEMENT_3D ( 'NONE', #15515, #4436, #17421 ) ;
#8848 = CARTESIAN_POINT ( 'NONE',  ( -8.190968255476823501, 42.92868192021149554, 75.86215881574817388 ) ) ;
#8849 = DIRECTION ( 'NONE',  ( 1.000000000000000000, 0.000000000000000000, 0.000000000000000000 ) ) ;
#8850 = EDGE_CURVE ( 'NONE', #14271, #12459, #8987, .T. ) ;
#8851 = CARTESIAN_POINT ( 'NONE',  ( -0.8303902511565894873, 52.85771897673274111, 78.94509925486606505 ) ) ;
#8852 = CARTESIAN_POINT ( 'NONE',  ( -5.154188915835984375, 42.64120994080404614, 92.21121380123797451 ) ) ;
#8853 = ADVANCED_FACE ( 'NONE', ( #13975 ), #7372, .F. ) ;
#8854 = CARTESIAN_POINT ( 'NONE',  ( -6.962266735612947066, 47.40375324003255741, 78.31366413292410300 ) ) ;
#8855 = CARTESIAN_POINT ( 'NONE',  ( -3.350035803220276609, 49.20851703305431357, 95.72683880123798872 ) ) ;
#8856 = VECTOR ( 'NONE', #11191, 999.9999999999998863 ) ;
#8857 = PRODUCT_DEFINITION ( 'UNKNOWN', '', #2409, #8266 ) ;
#8858 = DIRECTION ( 'NONE',  ( 1.000000000000000000, -1.110223024625156540E-16, 1.779391786395883043E-16 ) ) ;
#8859 = ORIENTED_EDGE ( 'NONE', *, *, #2214, .F. ) ;
#8860 = ADVANCED_FACE ( 'NONE', ( #4181 ), #17575, .F. ) ;
#8861 = CARTESIAN_POINT ( 'NONE',  ( 1.485376517908854721, 52.30695239789775997, 75.48605119142476383 ) ) ;
#8862 = ORIENTED_EDGE ( 'NONE', *, *, #20534, .F. ) ;
#8863 = VECTOR ( 'NONE', #5357, 1000.000000000000000 ) ;
#8864 = CARTESIAN_POINT ( 'NONE',  ( 2.259191861956070024, 47.76843358786783966, 77.41730067788147096 ) ) ;
#8865 =( REPRESENTATION_RELATIONSHIP ('NONE','NONE', #11365, #9739 ) REPRESENTATION_RELATIONSHIP_WITH_TRANSFORMATION ( #7719 )SHAPE_REPRESENTATION_RELATIONSHIP( ) );
#8866 = CARTESIAN_POINT ( 'NONE',  ( -0.3080929418689875576, 37.85583172076933778, 92.44558880123798872 ) ) ;
#8867 = EDGE_LOOP ( 'NONE', ( #10147, #6408 ) ) ;
#8868 = CARTESIAN_POINT ( 'NONE',  ( 4.673174852049361228, 39.63213674411673537, 94.36058879782399345 ) ) ;
#8869 = CARTESIAN_POINT ( 'NONE',  ( 0.5915428171209280439, 52.96190779654647685, 77.38375056423674891 ) ) ;
#8870 = CARTESIAN_POINT ( 'NONE',  ( -3.350758615681482144, 52.21051221579373447, 78.23748737924660190 ) ) ;
#8871 = CARTESIAN_POINT ( 'NONE',  ( 0.7375380209976891699, 52.95956711614144297, 77.42541598925475910 ) ) ;
#8872 = CARTESIAN_POINT ( 'NONE',  ( 5.633915549615357676, 51.32674344226200702, 77.24912405724838038 ) ) ;
#8873 = CARTESIAN_POINT ( 'NONE',  ( -7.600593896485818846, 45.28511094584521146, 72.45433879953085921 ) ) ;
#8874 = ORIENTED_EDGE ( 'NONE', *, *, #17335, .F. ) ;
#8875 = PRODUCT_DEFINITION_FORMATION_WITH_SPECIFIED_SOURCE ( 'ANY', '', #10609, .NOT_KNOWN. ) ;
#8876 = CARTESIAN_POINT ( 'NONE',  ( 8.286596668832688195, 41.52487556862202922, 77.52280427046368061 ) ) ;
#8877 = VERTEX_POINT ( 'NONE', #19480 ) ;
#8878 = CARTESIAN_POINT ( 'NONE',  ( 6.352353975415561571, 49.92870928545907816, 77.86676136243460178 ) ) ;
#8879 = PLANE ( 'NONE',  #20936 ) ;
#8880 = FACE_OUTER_BOUND ( 'NONE', #3998, .T. ) ;
#8881 = CARTESIAN_POINT ( 'NONE',  ( 6.828503391016846891, 43.33193468930419101, 92.91433880123800293 ) ) ;
#8882 = DIRECTION ( 'NONE',  ( 0.02533578529877050789, 0.9996789974703352843, 1.831801750099146688E-16 ) ) ;
#8883 = CARTESIAN_POINT ( 'NONE',  ( 4.155789158466160593, 39.80095668645486029, 95.44472199408899371 ) ) ;
#8884 = EDGE_CURVE ( 'NONE', #4878, #5410, #18302, .T. ) ;
#8885 = CARTESIAN_POINT ( 'NONE',  ( -5.056163503743585252, 37.34224500634140043, 75.38158877174898009 ) ) ;
#8886 = ORIENTED_EDGE ( 'NONE', *, *, #13038, .T. ) ;
#8887 = EDGE_CURVE ( 'NONE', #3265, #895, #9817, .T. ) ;
#8888 = CARTESIAN_POINT ( 'NONE',  ( -0.7567330459223939876, 36.05414901439895914, 77.72082377648446538 ) ) ;
#8889 = VECTOR ( 'NONE', #1933, 1000.000000000000114 ) ;
#8890 = ORIENTED_EDGE ( 'NONE', *, *, #555, .T. ) ;
#8891 = DIRECTION ( 'NONE',  ( 0.7071067811865433539, -0.7071067811865517916, 1.146387601258590612E-16 ) ) ;
#8892 = CARTESIAN_POINT ( 'NONE',  ( 1.868012774839550749, 39.13936707477651566, 95.57058879953099506 ) ) ;
#8893 = CARTESIAN_POINT ( 'NONE',  ( -2.904223097202481174, 48.62752260303690122, 91.27371379953098085 ) ) ;
#8894 = B_SPLINE_SURFACE_WITH_KNOTS ( 'NONE', 3, 1, ( 
 ( #6567, #12755 ),
 ( #16372, #4862 ),
 ( #9996, #14765 ),
 ( #186, #17854 ),
 ( #9685, #19234 ),
 ( #3279, #3375 ),
 ( #17753, #16263 ),
 ( #16061, #9891 ),
 ( #7970, #17960 ),
 ( #17638, #18066 ),
 ( #1691, #1587 ) ),
 .UNSPECIFIED., .F., .F., .F.,
 ( 4, 1, 1, 1, 1, 1, 1, 1, 4 ),
 ( 2, 2 ),
 ( 0.000000000000000000, 0.1230989878275519644, 0.2403818709996815850, 0.3547287725962395277, 0.4701889909135318901, 0.5896219003167558759, 0.7153806559642975627, 0.8522030906580475573, 1.000000000000000000 ),
 ( 0.000000000000000000, 1.000000000000000000 ),
 .UNSPECIFIED. ) ;
#8895 = CARTESIAN_POINT ( 'NONE',  ( -7.250832141565055622, 41.98755119451053730, 77.57193099691271243 ) ) ;
#8896 = ORIENTED_EDGE ( 'NONE', *, *, #16127, .F. ) ;
#8897 = CARTESIAN_POINT ( 'NONE',  ( -5.154188915835984375, 42.64120994080404614, 92.36746380123797451 ) ) ;
#8898 = CARTESIAN_POINT ( 'NONE',  ( 0.5915428171209280439, 52.96190779654647685, 77.38375056423674891 ) ) ;
#8899 = CARTESIAN_POINT ( 'NONE',  ( -3.117807152840563756, 40.03267073656082431, 95.05433879953105247 ) ) ;
#8900 = DIRECTION ( 'NONE',  ( 0.8660254037844395958, -0.4999999999999985012, 0.000000000000000000 ) ) ;
#8901 = VERTEX_POINT ( 'NONE', #7792 ) ;
#8902 = FACE_BOUND ( 'NONE', #18328, .T. ) ;
#8903 = CARTESIAN_POINT ( 'NONE',  ( 6.828503391016846891, 43.33193468930419101, 95.41433880123797451 ) ) ;
#8904 = AXIS2_PLACEMENT_3D ( 'NONE', #2961, #14351, #9574 ) ;
#8905 = ORIENTED_EDGE ( 'NONE', *, *, #9488, .T. ) ;
#8906 = CARTESIAN_POINT ( 'NONE',  ( 0.5221537403065109606, 50.16218137147969713, 51.55433879953100273 ) ) ;
#8907 = CARTESIAN_POINT ( 'NONE',  ( 30.92220646078100188, 42.76218137147968434, 62.80715055817104542 ) ) ;
#8908 = VECTOR ( 'NONE', #946, 1000.000000000000000 ) ;
#8909 = ITEM_DEFINED_TRANSFORMATION ( 'NONE', 'NONE', #1051,  #18366 ) ;
#8910 = CARTESIAN_POINT ( 'NONE',  ( 8.378637954445377289, 41.81363803720061867, 72.45433879953087342 ) ) ;
#8911 = CARTESIAN_POINT ( 'NONE',  ( 0.5398981455733474766, 52.96229826333378554, 78.93477474516929249 ) ) ;
#8912 = PLANE ( 'NONE',  #13325 ) ;
#8913 = EDGE_LOOP ( 'NONE', ( #16647, #18049, #8874, #13961 ) ) ;
#8914 = CARTESIAN_POINT ( 'NONE',  ( 1.932080035760362247, 52.95579814665390472, 75.81376357423876300 ) ) ;
#8915 = EDGE_LOOP ( 'NONE', ( #4983, #11875, #13765, #2181 ) ) ;
#8916 = AXIS2_PLACEMENT_3D ( 'NONE', #5949, #4028, #12038 ) ;
#8917 = CARTESIAN_POINT ( 'NONE',  ( 6.955656837306707807, 50.35042639603116044, 76.39262467917644983 ) ) ;
#8918 = DIRECTION ( 'NONE',  ( 0.9534635866061452747, 0.3015081906286224411, 2.009271279954815304E-16 ) ) ;
#8919 = CARTESIAN_POINT ( 'NONE',  ( -0.9988176903691428077, 49.83852402762217082, 95.80496380123798872 ) ) ;
#8920 = EDGE_LOOP ( 'NONE', ( #3767, #17605, #7462, #82 ) ) ;
#8921 = DIRECTION ( 'NONE',  ( -0.9999689119394086223, 0.007885122365275665235, -1.526048693634353392E-16 ) ) ;
#8922 = VERTEX_POINT ( 'NONE', #11315 ) ;
#8923 = CARTESIAN_POINT ( 'NONE',  ( 5.018290002877273892, 50.86746622949960539, 79.53290755650829169 ) ) ;
#8924 = CARTESIAN_POINT ( 'NONE',  ( -1.183761187420877548, 49.81017696809242068, 92.55433879953098142 ) ) ;
#8925 = CARTESIAN_POINT ( 'NONE',  ( 2.891178764483326002, 49.58011693221236271, 93.01356103993782654 ) ) ;
#8926 = DIRECTION ( 'NONE',  ( -1.540237394707284467E-16, -1.793354297423764243E-16, 1.000000000000000000 ) ) ;
#8927 = LINE ( 'NONE', #18495, #17086 ) ;
#8928 = CARTESIAN_POINT ( 'NONE',  ( 5.611423337425062385, 41.22389019960463230, 94.08621380123797451 ) ) ;
#8929 = CARTESIAN_POINT ( 'NONE',  ( 0.8251303722654924622, 52.35233671442713899, 77.55588632845071118 ) ) ;
#8931 = CARTESIAN_POINT ( 'NONE',  ( 31.07218010054375412, 42.76218137147968434, 70.80574467885102763 ) ) ;
#8930 = AXIS2_PLACEMENT_3D ( 'NONE', #16198, #20654, #19273 ) ;
#8932 = CARTESIAN_POINT ( 'NONE',  ( 5.722153740306476166, 44.16218185472587976, 94.89411094854372664 ) ) ;
#8933 = CARTESIAN_POINT ( 'NONE',  ( 6.102441102155617969, 43.42752260303680600, 94.86746380294499659 ) ) ;
#8934 = VECTOR ( 'NONE', #15460, 1000.000000000000000 ) ;
#8935 = CARTESIAN_POINT ( 'NONE',  ( -7.956935296483398368, 41.77702279339499825, 78.50654468188380974 ) ) ;
#8936 = CARTESIAN_POINT ( 'NONE',  ( 8.787829143201870252, 41.13140593384865440, 76.40801527011910821 ) ) ;
#8937 = CARTESIAN_POINT ( 'NONE',  ( 0.5221537403065188432, 44.16218137147969003, 54.55433879953099563 ) ) ;
#8938 = PLANE ( 'NONE',  #13690 ) ;
#8939 = CARTESIAN_POINT ( 'NONE',  ( 6.102441102155617969, 43.42752260303680600, 90.80496379953099506 ) ) ;
#8940 = VECTOR ( 'NONE', #1425, 1000.000000000000114 ) ;
#8941 = CARTESIAN_POINT ( 'NONE',  ( -7.677846259693480668, 36.96218137147968008, 53.35433879953099989 ) ) ;
#8942 = CARTESIAN_POINT ( 'NONE',  ( -7.857211665749059826, 46.86741566905539713, 79.32924967153994089 ) ) ;
#8943 = CARTESIAN_POINT ( 'NONE',  ( 2.263811127080452845, 49.90383875825364157, 77.41268141275706682 ) ) ;
#8944 = EDGE_CURVE ( 'NONE', #13012, #13982, #957, .T. ) ;
#8945 = FACE_OUTER_BOUND ( 'NONE', #12190, .T. ) ;
#8946 = ORIENTED_EDGE ( 'NONE', *, *, #19352, .T. ) ;
#8947 = PRODUCT_DEFINITION_CONTEXT ( 'detailed design', #5175, 'design' ) ;
#8948 = CARTESIAN_POINT ( 'NONE',  ( 8.569783991210568885, 42.84232883131717529, 79.15097751326614173 ) ) ;
#8949 = CARTESIAN_POINT ( 'NONE',  ( 30.92220646078100188, 42.96218137147968008, 57.80715055817105252 ) ) ;
#8950 = PLANE ( 'NONE',  #18770 ) ;
#8951 = B_SPLINE_CURVE_WITH_KNOTS ( 'NONE', 3,
 ( #11060, #6449, #1681, #20610, #17845, #14443, #9568, #16154, #12748, #4641, #11374, #7958, #12955, #2953, #4742, #19434, #21014, #17432, #14343, #17741, #20818, #9357, #6246 ),
 .UNSPECIFIED., .F., .F.,
 ( 4, 1, 1, 1, 1, 1, 1, 1, 1, 1, 1, 1, 1, 1, 1, 1, 1, 1, 1, 1, 4 ),
 ( 0.000000000000000000, 0.04683093660151300269, 0.09055667580802433114, 0.1312013806050136844, 0.1681729499244319359, 0.2024082766003676426, 0.2330515569695218725, 0.2607881417524846590, 0.2857054801288026469, 0.3326652789510584074, 0.3814982805224741425, 0.4333318279156733732, 0.4889629060548432160, 0.5467408684218817427, 0.6046224851005120859, 0.6645427963802341687, 0.7261481924644412889, 0.7902890061914499276, 0.8570127982043956871, 0.9269126820953633716, 1.000000000000000000 ),
 .UNSPECIFIED. ) ;
#8952 = CARTESIAN_POINT ( 'NONE',  ( -4.524181921268124462, 40.28999182795290324, 94.94558880123797451 ) ) ;
#8953 = LINE ( 'NONE', #15337, #2642 ) ;
#8954 = B_SPLINE_CURVE_WITH_KNOTS ( 'NONE', 3,
 ( #3464, #8149, #9975, #8580, #15064, #477, #11673, #12944, #14639, #3355, #1876 ),
 .UNSPECIFIED., .F., .F.,
 ( 4, 1, 1, 1, 1, 1, 1, 1, 4 ),
 ( 0.000000000000000000, 0.2096989846417539882, 0.3830033715279665407, 0.5180517223345033617, 0.6192761841629320640, 0.7029005363942016915, 0.7892332632667665715, 0.8867012962659018838, 1.000000000000000000 ),
 .UNSPECIFIED. ) ;
#8955 = CARTESIAN_POINT ( 'NONE',  ( 9.106328434870372135, 42.08596851619746104, 78.11626675975762168 ) ) ;
#8956 = CARTESIAN_POINT ( 'NONE',  ( -0.8237052942265477018, 49.18499566818285018, 91.50808880294498238 ) ) ;
#8957 = CARTESIAN_POINT ( 'NONE',  ( -4.412197277429617870, 51.45204700985827628, 76.06958028623719770 ) ) ;
#8958 = VECTOR ( 'NONE', #11936, 1000.000000000000000 ) ;
#8959 = EDGE_CURVE ( 'NONE', #6196, #19924, #16506, .T. ) ;
#8960 = CARTESIAN_POINT ( 'NONE',  ( -7.088677424969694663, 47.02489238468576360, 77.68791732120209304 ) ) ;
#8961 = CARTESIAN_POINT ( 'NONE',  ( 6.828503391016846891, 43.33193468930419101, 90.25808880123800293 ) ) ;
#8962 = CARTESIAN_POINT ( 'NONE',  ( 6.814395614697851933, 37.84261482370956031, 75.97427057108799886 ) ) ;
#8963 = VERTEX_POINT ( 'NONE', #8003 ) ;
#8964 = CARTESIAN_POINT ( 'NONE',  ( 5.924340528221679669, 51.11221820959726614, 77.13671500005938242 ) ) ;
#8965 = EDGE_CURVE ( 'NONE', #8763, #19237, #14489, .T. ) ;
#8966 = ORIENTED_EDGE ( 'NONE', *, *, #9457, .T. ) ;
#8967 = PLANE ( 'NONE',  #3730 ) ;
#8968 = CARTESIAN_POINT ( 'NONE',  ( -5.154188915835984375, 42.64120994080404614, 90.96121380123797451 ) ) ;
#8969 = ORIENTED_EDGE ( 'NONE', *, *, #12127, .T. ) ;
#8970 = ADVANCED_FACE ( 'NONE', ( #11416 ), #4793, .F. ) ;
#8971 = DIRECTION ( 'NONE',  ( -0.8136266022444372803, -0.5813877811927011807, -2.295812393977109100E-16 ) ) ;
#8972 = EDGE_CURVE ( 'NONE', #15539, #15079, #12899, .T. ) ;
#8973 = VECTOR ( 'NONE', #6261, 1000.000000000000000 ) ;
#8974 = CARTESIAN_POINT ( 'NONE',  ( -3.165193363162642104, 51.42333476898780020, 79.18928797456808866 ) ) ;
#8975 = LINE ( 'NONE', #773, #265 ) ;
#8976 = FACE_OUTER_BOUND ( 'NONE', #20065, .T. ) ;
#8977 = CARTESIAN_POINT ( 'NONE',  ( 6.961907239250668233, 50.34580947589670075, 76.63889762306028786 ) ) ;
#8978 = ORIENTED_EDGE ( 'NONE', *, *, #6506, .F. ) ;
#8979 = DIRECTION ( 'NONE',  ( 1.402518428993831676E-16, -1.000000000000000000, 1.677918375355662166E-32 ) ) ;
#8980 = CARTESIAN_POINT ( 'NONE',  ( 5.666884522201895535, 41.76315400873614436, 93.03246379782397923 ) ) ;
#8981 = ORIENTED_EDGE ( 'NONE', *, *, #5746, .F. ) ;
#8982 = CARTESIAN_POINT ( 'NONE',  ( 2.522153740306511960, 47.62628298661745418, 45.55433879953100273 ) ) ;
#8983 = CARTESIAN_POINT ( 'NONE',  ( 4.540095451430588902, 52.13470428702989068, 76.74217282813371810 ) ) ;
#8984 = CARTESIAN_POINT ( 'NONE',  ( 7.864691922653266332, 47.81281597943210215, 78.56977997600147035 ) ) ;
#8985 = ADVANCED_FACE ( 'NONE', ( #2999 ), #15474, .F. ) ;
#8986 = CARTESIAN_POINT ( 'NONE',  ( 6.885459498894642927, 50.40227834219487590, 78.84682786933051091 ) ) ;
#8987 = LINE ( 'NONE', #886, #4352 ) ;
#8988 = CARTESIAN_POINT ( 'NONE',  ( 5.839584039462725862, 37.14605016217623046, 76.11636564480957645 ) ) ;
#8989 = CARTESIAN_POINT ( 'NONE',  ( -4.716387082485073989, 37.09126585098686490, 75.36022115247205022 ) ) ;
#8990 = ORIENTED_EDGE ( 'NONE', *, *, #5810, .T. ) ;
#8991 = CARTESIAN_POINT ( 'NONE',  ( 8.787893756631275366, 41.13159958439556618, 78.49453464888588883 ) ) ;
#8992 = VERTEX_POINT ( 'NONE', #2146 ) ;
#8993 = CARTESIAN_POINT ( 'NONE',  ( -3.952897528319690323, 50.86047021225675024, 75.37146543928014353 ) ) ;
#8994 = CARTESIAN_POINT ( 'NONE',  ( -0.8237052942265477018, 49.18499566818285018, 96.19558879953099506 ) ) ;
#8995 = CARTESIAN_POINT ( 'NONE',  ( -8.178850963866057810, 42.47164029129891105, 76.61471288230795551 ) ) ;
#8996 = EDGE_LOOP ( 'NONE', ( #15582, #4885, #15186, #401 ) ) ;
#8997 = ADVANCED_FACE ( 'NONE', ( #18305 ), #16990, .F. ) ;
#8998 = CARTESIAN_POINT ( 'NONE',  ( -3.350035803220276609, 49.20851703305431357, 94.63308880123798872 ) ) ;
#8999 = CARTESIAN_POINT ( 'NONE',  ( -1.876873622437040590, 39.01745058958429269, 95.21996379782397923 ) ) ;
#9000 = CARTESIAN_POINT ( 'NONE',  ( -5.154188915835984375, 42.64120994080404614, 94.71121380123804556 ) ) ;
#9001 = ORIENTED_EDGE ( 'NONE', *, *, #10962, .T. ) ;
#9002 = CARTESIAN_POINT ( 'NONE',  ( 5.288291328326708118, 36.75211657491283290, 75.39318197153889400 ) ) ;
#9003 = DIRECTION ( 'NONE',  ( -1.571217453038212812E-16, -0.7071067811865500152, -0.7071067811865451302 ) ) ;
#9004 = EDGE_CURVE ( 'NONE', #20977, #6883, #11860, .T. ) ;
#9005 = VERTEX_POINT ( 'NONE', #325 ) ;
#9006 = CARTESIAN_POINT ( 'NONE',  ( 1.847086472663199253, 52.25482134247464927, 79.19213266016700459 ) ) ;
#9007 = CARTESIAN_POINT ( 'NONE',  ( 1.352400422481993658, 50.46853102219002096, 91.97683880123797451 ) ) ;
#9008 = ORIENTED_EDGE ( 'NONE', *, *, #10262, .F. ) ;
#9009 = CARTESIAN_POINT ( 'NONE',  ( -4.633747169617723927, 50.53922380117749213, 79.50315915470658013 ) ) ;
#9010 = DIRECTION ( 'NONE',  ( 1.402518428993831676E-16, -1.000000000000000000, 0.000000000000000000 ) ) ;
#9011 = EDGE_CURVE ( 'NONE', #17415, #17446, #860, .T. ) ;
#9012 = CARTESIAN_POINT ( 'NONE',  ( 3.122075258343615545, 38.59543968120053847, 90.05576841395854615 ) ) ;
#9013 = EDGE_CURVE ( 'NONE', #8877, #15717, #7452, .T. ) ;
#9014 = APPLICATION_PROTOCOL_DEFINITION ( 'draft international standard', 'automotive_design', 1998, #1243 ) ;
#9015 = DIRECTION ( 'NONE',  ( -1.540237394707284220E-16, -1.793354297423764243E-16, 1.000000000000000000 ) ) ;
#9016 = CARTESIAN_POINT ( 'NONE',  ( 5.245411638781020791, 50.86060015470197726, 78.76051003739772227 ) ) ;
#9017 = CARTESIAN_POINT ( 'NONE',  ( -5.368445182934975968, 51.36218137147968577, 93.55433879953098142 ) ) ;
#9018 = EDGE_LOOP ( 'NONE', ( #3459, #19599, #1967, #1299, #4735, #334, #11264, #13388, #3347, #5755, #5365, #18761 ) ) ;
#9019 = CARTESIAN_POINT ( 'NONE',  ( 2.120607010463642528, 52.95431154217356351, 76.45922371407752394 ) ) ;
#9020 = ORIENTED_EDGE ( 'NONE', *, *, #17009, .T. ) ;
#9021 = CARTESIAN_POINT ( 'NONE',  ( 2.522153740306504854, 47.62628298661744708, 85.15433879953098995 ) ) ;
#9022 = CARTESIAN_POINT ( 'NONE',  ( 0.3279354642263507258, 52.35625727899917337, 77.76169174070734869 ) ) ;
#9023 = CARTESIAN_POINT ( 'NONE',  ( -5.154188915835984375, 42.64120994080404614, 94.71121380123797451 ) ) ;
#9024 = ORIENTED_EDGE ( 'NONE', *, *, #3836, .T. ) ;
#9025 = FACE_OUTER_BOUND ( 'NONE', #16184, .T. ) ;
#9026 = ORIENTED_EDGE ( 'NONE', *, *, #8319, .F. ) ;
#9027 = CARTESIAN_POINT ( 'NONE',  ( 4.772654808018759631, 51.96292205838052070, 79.19424447893550223 ) ) ;
#9028 = CARTESIAN_POINT ( 'NONE',  ( -1.477846259693493813, 49.81903562097207327, 77.15433879953100416 ) ) ;
#9029 = CARTESIAN_POINT ( 'NONE',  ( 8.395197883163783459, 39.95466513945179798, 76.21925085218815354 ) ) ;
#9030 = CARTESIAN_POINT ( 'NONE',  ( -4.525688498162968365, 36.95040448855567661, 78.17872471894986575 ) ) ;
#9031 = CARTESIAN_POINT ( 'NONE',  ( -6.771957287108766543, 40.50912055441206405, 79.09912640779528203 ) ) ;
#9032 = DIRECTION ( 'NONE',  ( 1.540237394707284220E-16, 1.793354297423764243E-16, -1.000000000000000000 ) ) ;
#9033 = EDGE_CURVE ( 'NONE', #19399, #16713, #9060, .T. ) ;
#9034 = CARTESIAN_POINT ( 'NONE',  ( -2.416137431568557314, 39.07291177436112406, 96.27371380123797451 ) ) ;
#9035 = CARTESIAN_POINT ( 'NONE',  ( 0.5221537403065064087, 48.16218137147969003, 69.55433879953100984 ) ) ;
#9036 = CARTESIAN_POINT ( 'NONE',  ( -5.390530271885531022, 49.83319048879877045, 76.36675183022860836 ) ) ;
#9037 = CARTESIAN_POINT ( 'NONE',  ( 4.826069222465897646, 51.92346698209227895, 75.62563104034643402 ) ) ;
#9038 = CARTESIAN_POINT ( 'NONE',  ( 3.948530577815480225, 39.69684013992245752, 90.96121380294498238 ) ) ;
#9039 = CARTESIAN_POINT ( 'NONE',  ( -7.291677074388141833, 40.11445521940208891, 78.59658243778928011 ) ) ;
#9040 = ORIENTED_EDGE ( 'NONE', *, *, #4775, .F. ) ;
#9041 = CARTESIAN_POINT ( 'NONE',  ( 8.934486310075088866, 41.57094676672487310, 78.86350455626283917 ) ) ;
#9042 = FACE_OUTER_BOUND ( 'NONE', #11672, .T. ) ;
#9043 = PLANE ( 'NONE',  #5838 ) ;
#9044 = CARTESIAN_POINT ( 'NONE',  ( -3.350053155021378792, 52.21101631215288563, 78.15066919019970726 ) ) ;
#9045 = LINE ( 'NONE', #13931, #15374 ) ;
#9046 = CARTESIAN_POINT ( 'NONE',  ( -4.529265440370440210, 36.95304663167631531, 77.01245883157920957 ) ) ;
#9047 = CARTESIAN_POINT ( 'NONE',  ( -7.465715295087656855, 42.67411418385548671, 79.33973788556694728 ) ) ;
#9048 = CARTESIAN_POINT ( 'NONE',  ( 8.641107047301593624, 43.01204830781416888, 77.56292432728525910 ) ) ;
#9049 = EDGE_CURVE ( 'NONE', #19214, #11104, #18839, .T. ) ;
#9050 = CARTESIAN_POINT ( 'NONE',  ( -4.616992131696503243, 37.01784680471218536, 75.99117330331094422 ) ) ;
#9051 = ORIENTED_EDGE ( 'NONE', *, *, #20629, .T. ) ;
#9052 = CARTESIAN_POINT ( 'NONE',  ( 8.025069409823680999, 40.85162907203753946, 75.45988996333271359 ) ) ;
#9053 = DIRECTION ( 'NONE',  ( -0.3165065846431825980, -0.9485903129789530208, 0.000000000000000000 ) ) ;
#9054 = DIRECTION ( 'NONE',  ( -1.193617070626243484E-16, -1.000000000000000000, -0.000000000000000000 ) ) ;
#9055 = CARTESIAN_POINT ( 'NONE',  ( 2.263811127080455954, 49.90383875825364157, 53.41268141275705972 ) ) ;
#9056 = SHAPE_REPRESENTATION ( 'Bushing', ( #18366 ), #17679 ) ;
#9057 = CARTESIAN_POINT ( 'NONE',  ( 5.748274343403736886, 51.24227120794373747, 77.94845644658968808 ) ) ;
#9058 = FACE_OUTER_BOUND ( 'NONE', #4623, .T. ) ;
#9059 = CARTESIAN_POINT ( 'NONE',  ( 4.613683985508550300, 40.84891963687440608, 89.75946567728124137 ) ) ;
#9060 = LINE ( 'NONE', #15443, #15603 ) ;
#9061 = AXIS2_PLACEMENT_3D ( 'NONE', #4369, #15784, #11098 ) ;
#9062 = CARTESIAN_POINT ( 'NONE',  ( -1.477846259693496922, 49.81903562097207327, 51.21119304902337888 ) ) ;
#9063 = CARTESIAN_POINT ( 'NONE',  ( 5.568489401881125289, 48.03437091500646261, 91.66433880123796030 ) ) ;
#9064 = ADVANCED_FACE ( 'NONE', ( #754 ), #20636, .T. ) ;
#9065 = CARTESIAN_POINT ( 'NONE',  ( 6.866536783559561208, 37.87987299396810670, 76.25518385353585415 ) ) ;
#9066 = ORIENTED_EDGE ( 'NONE', *, *, #2976, .T. ) ;
#9067 = CARTESIAN_POINT ( 'NONE',  ( 5.755371611800503828, 51.23702874167446453, 77.28963291717792572 ) ) ;
#9068 = VERTEX_POINT ( 'NONE', #15341 ) ;
#9069 = CARTESIAN_POINT ( 'NONE',  ( -4.443144554159853321, 50.68301778673873059, 78.71090438869831019 ) ) ;
#9070 = CARTESIAN_POINT ( 'NONE',  ( -2.904223097202481174, 48.62752260303690122, 92.83621380294498238 ) ) ;
#9071 = VERTEX_POINT ( 'NONE', #7239 ) ;
#9072 = CARTESIAN_POINT ( 'NONE',  ( -3.476578273656611984, 48.74765469743772428, 94.98020409461689439 ) ) ;
#9073 = EDGE_CURVE ( 'NONE', #13698, #15976, #17441, .T. ) ;
#9074 = CARTESIAN_POINT ( 'NONE',  ( -7.677846259693484221, 36.96218137147968008, 53.35433879953099989 ) ) ;
#9075 = VECTOR ( 'NONE', #14924, 1000.000000000000000 ) ;
#9076 = EDGE_CURVE ( 'NONE', #11628, #9753, #11108, .T. ) ;
#9077 = CARTESIAN_POINT ( 'NONE',  ( -3.746334366659155979, 51.00807268481932510, 79.50772166908967620 ) ) ;
#9078 = LINE ( 'NONE', #875, #7750 ) ;
#9079 = FACE_OUTER_BOUND ( 'NONE', #3234, .T. ) ;
#9080 = CARTESIAN_POINT ( 'NONE',  ( -3.874372605692208094, 36.46930367539203388, 79.33401574558745040 ) ) ;
#9081 = ORIENTED_EDGE ( 'NONE', *, *, #14019, .T. ) ;
#9082 = CARTESIAN_POINT ( 'NONE',  ( 6.522436035574397550, 49.75115376156129798, 72.45433879953087342 ) ) ;
#9083 = CARTESIAN_POINT ( 'NONE',  ( 5.856396280011940014, 46.10368687828906076, 93.18871379782397923 ) ) ;
#9084 = ORIENTED_EDGE ( 'NONE', *, *, #2977, .F. ) ;
#9085 = ADVANCED_BREP_SHAPE_REPRESENTATION ( '', ( #11671, #18366 ), #9896 ) ;
#9086 = FACE_OUTER_BOUND ( 'NONE', #17351, .T. ) ;
#9087 = CARTESIAN_POINT ( 'NONE',  ( 6.545534159973747990, 50.65336749702785113, 77.68963291717794561 ) ) ;
#9088 = CARTESIAN_POINT ( 'NONE',  ( 6.828503391016846891, 43.33193468930419101, 95.25808880123800293 ) ) ;
#9089 = CARTESIAN_POINT ( 'NONE',  ( -6.647464070959230753, 48.14170149837704571, 72.45433879953087342 ) ) ;
#9090 = DIRECTION ( 'NONE',  ( -0.9534635866061452747, -0.3015081906286225522, -2.009271279954815797E-16 ) ) ;
#9091 = CARTESIAN_POINT ( 'NONE',  ( 31.22215374030650281, 45.56218137147968861, 72.80433879953100984 ) ) ;
#9092 = CONICAL_SURFACE ( 'NONE', #20945, 6.200000000000020606, 1.047197551196600518 ) ;
#9093 = VERTEX_POINT ( 'NONE', #18525 ) ;
#9094 = CARTESIAN_POINT ( 'NONE',  ( 4.100647748703544870, 51.54014729097003311, 76.70496318590288354 ) ) ;
#9095 = ORIENTED_EDGE ( 'NONE', *, *, #18588, .T. ) ;
#9096 = CARTESIAN_POINT ( 'NONE',  ( -4.472548095981605520, 51.40892252450552036, 75.36471306604558151 ) ) ;
#9097 = CARTESIAN_POINT ( 'NONE',  ( -5.058133621542618030, 44.89684013992257405, 91.42996379953099506 ) ) ;
#9098 = ORIENTED_EDGE ( 'NONE', *, *, #7398, .T. ) ;
#9099 = CARTESIAN_POINT ( 'NONE',  ( 4.394343283833276992, 39.11584570990505938, 95.25808880123800293 ) ) ;
#9100 = CARTESIAN_POINT ( 'NONE',  ( 4.155795601789611382, 39.80096205483764038, 95.44472229536860652 ) ) ;
#9101 = CARTESIAN_POINT ( 'NONE',  ( 6.433553176315263578, 38.47928099333162777, 72.45433879953087342 ) ) ;
#9102 = ORIENTED_EDGE ( 'NONE', *, *, #19345, .F. ) ;
#9103 = VECTOR ( 'NONE', #10354, 1000.000000000000000 ) ;
#9104 = CARTESIAN_POINT ( 'NONE',  ( 9.176231272041631470, 45.98187388689780164, 75.44992703482499508 ) ) ;
#9105 = EDGE_CURVE ( 'NONE', #10886, #16595, #7285, .T. ) ;
#9106 = FACE_OUTER_BOUND ( 'NONE', #14457, .T. ) ;
#9107 = ORIENTED_EDGE ( 'NONE', *, *, #6887, .T. ) ;
#9108 = DIRECTION ( 'NONE',  ( 3.620524460287510065E-17, -1.000000000000000000, -7.183611964723545059E-17 ) ) ;
#9109 = CARTESIAN_POINT ( 'NONE',  ( 6.198496396448986090, 45.68315280215533392, 90.49246380123798872 ) ) ;
#9110 = COLOUR_RGB ( '', 0.40784314, 0.44705882, 0.49803922) ;
#9111 = VERTEX_POINT ( 'NONE', #2113 ) ;
#9112 = CARTESIAN_POINT ( 'NONE',  ( -5.195654067311837210, 50.04042785407680327, 79.16788338592567698 ) ) ;
#9113 = CARTESIAN_POINT ( 'NONE',  ( 5.110857744515833190, 37.36631113118844638, 76.10944558133218152 ) ) ;
#9114 = CARTESIAN_POINT ( 'NONE',  ( 3.460444912181559474, 49.25145096859824889, 91.74246380123798872 ) ) ;
#9115 = ITEM_DEFINED_TRANSFORMATION ( 'NONE', 'NONE', #10231,  #18366 ) ;
#9116 = CARTESIAN_POINT ( 'NONE',  ( -3.716800330428157384, 36.35291138305289849, 77.85659439586764563 ) ) ;
#9118 = ADVANCED_FACE ( 'NONE', ( #8388 ), #14870, .F. ) ;
#9117 = CARTESIAN_POINT ( 'NONE',  ( 5.478721299898049679, 36.88819086051147167, 76.06572720930677178 ) ) ;
#9119 = CARTESIAN_POINT ( 'NONE',  ( -7.609845089999874190, 43.10833364818387992, 76.06610350541322418 ) ) ;
#9120 = EDGE_CURVE ( 'NONE', #559, #8246, #17683, .T. ) ;
#9121 = ORIENTED_EDGE ( 'NONE', *, *, #17025, .T. ) ;
#9122 = FACE_OUTER_BOUND ( 'NONE', #7962, .T. ) ;
#9123 = ORIENTED_EDGE ( 'NONE', *, *, #8184, .T. ) ;
#9124 = CARTESIAN_POINT ( 'NONE',  ( -0.5095519206278340540, 52.29771471936252425, 79.29519679866520221 ) ) ;
#9125 = EDGE_CURVE ( 'NONE', #9436, #4858, #20473, .T. ) ;
#9126 = CARTESIAN_POINT ( 'NONE',  ( 2.522153740306505298, 50.16218137147969713, 83.55433879953099563 ) ) ;
#9127 = CARTESIAN_POINT ( 'NONE',  ( -3.350035803220276609, 49.20851703305431357, 94.47683880123798872 ) ) ;
#9128 = EDGE_CURVE ( 'NONE', #16684, #129, #16891, .T. ) ;
#9129 = ORIENTED_EDGE ( 'NONE', *, *, #8472, .T. ) ;
#9130 = CARTESIAN_POINT ( 'NONE',  ( -2.627048034785010699, 48.88511640015991588, 92.45433879952862810 ) ) ;
#9131 = EDGE_LOOP ( 'NONE', ( #12073, #11975, #17719, #13853, #9591, #6437, #19408, #8681, #13816, #6797, #20524, #15776, #3167, #19064, #12722, #11385, #13958, #5446, #12129, #20545, #12316, #18038, #17923, #5335 ) ) ;
#9132 = ADVANCED_FACE ( 'NONE', ( #16689 ), #402, .F. ) ;
#9133 = CARTESIAN_POINT ( 'NONE',  ( 2.522153740306498193, 49.81903562097208038, 123.5543387995310098 ) ) ;
#9134 = CYLINDRICAL_SURFACE ( 'NONE', #998, 8.199999999999999289 ) ;
#9135 = CARTESIAN_POINT ( 'NONE',  ( 8.387016861607721196, 39.93014609885396027, 76.70090004521539129 ) ) ;
#9136 = VECTOR ( 'NONE', #7034, 1000.000000000000000 ) ;
#9137 = VERTEX_POINT ( 'NONE', #18175 ) ;
#9138 = CARTESIAN_POINT ( 'NONE',  ( -4.990412171993358292, 37.29367714620271101, 77.90250793075740887 ) ) ;
#9139 = CARTESIAN_POINT ( 'NONE',  ( 5.884818748728627646, 51.14141135607439992, 78.06587361566768379 ) ) ;
#9140 = DIRECTION ( 'NONE',  ( 6.308085367188358884E-15, 0.000000000000000000, 1.000000000000000000 ) ) ;
#9141 = CARTESIAN_POINT ( 'NONE',  ( 30.92220646078100188, 42.76218137147968434, 62.80715055817104542 ) ) ;
#9142 = PLANE ( 'NONE',  #7387 ) ;
#9143 = CARTESIAN_POINT ( 'NONE',  ( -5.347586347461742662, 49.86387664491459049, 76.07566230427023868 ) ) ;
#9144 = CARTESIAN_POINT ( 'NONE',  ( 2.522153740306507963, 50.16218137147969713, 69.15433879953098995 ) ) ;
#9145 = CARTESIAN_POINT ( 'NONE',  ( -5.058133621542618030, 44.89684013992257405, 90.49246380294498238 ) ) ;
#9146 = LINE ( 'NONE', #9259, #19109 ) ;
#9147 = CARTESIAN_POINT ( 'NONE',  ( 8.951667845840693971, 41.62244091939069790, 78.41904468188381827 ) ) ;
#9148 = APPLICATION_CONTEXT ( 'automotive_design' ) ;
#9149 = VECTOR ( 'NONE', #13005, 1000.000000000000000 ) ;
#9150 = ORIENTED_EDGE ( 'NONE', *, *, #14442, .F. ) ;
#9151 = CARTESIAN_POINT ( 'NONE',  ( -7.611372734017124664, 43.12018948500615778, 75.45433879953087342 ) ) ;
#9152 = CARTESIAN_POINT ( 'NONE',  ( 0.5627506536433498630, 51.36208509089345142, 75.97198585835440099 ) ) ;
#9153 = EDGE_CURVE ( 'NONE', #11154, #5474, #19758, .T. ) ;
#9154 = CARTESIAN_POINT ( 'NONE',  ( -3.363202728395832342, 52.20162010845611178, 78.48078762820125576 ) ) ;
#9155 = CARTESIAN_POINT ( 'NONE',  ( 6.198496396448986090, 45.68315280215533392, 91.74246380123798872 ) ) ;
#9156 = CARTESIAN_POINT ( 'NONE',  ( 9.353817388681445522, 42.82770861117572281, 78.41904468188381827 ) ) ;
#9157 = CARTESIAN_POINT ( 'NONE',  ( -0.8111795930268366206, 49.49551470481303284, 85.82100546619767556 ) ) ;
#9158 = CARTESIAN_POINT ( 'NONE',  ( 5.430298293217690642, 36.85358955281711246, 77.55899030588862786 ) ) ;
#9159 = ORIENTED_EDGE ( 'NONE', *, *, #13892, .T. ) ;
#9160 = FACE_OUTER_BOUND ( 'NONE', #8136, .T. ) ;
#9161 = CARTESIAN_POINT ( 'NONE',  ( -4.092474520164236296, 50.94051422294817399, 76.01547346202475808 ) ) ;
#9162 = CARTESIAN_POINT ( 'NONE',  ( 0.3821786226492927541, 35.36301154328572949, 76.16022115247204738 ) ) ;
#9163 = CARTESIAN_POINT ( 'NONE',  ( 5.755371611800503828, 51.23702874167446453, 77.28963291717792572 ) ) ;
#9164 = CARTESIAN_POINT ( 'NONE',  ( 5.734785278855812685, 51.25223503655262647, 77.94915300234312383 ) ) ;
#9165 = VECTOR ( 'NONE', #18008, 1000.000000000000227 ) ;
#9166 = CARTESIAN_POINT ( 'NONE',  ( 9.242846470233811118, 42.49512172872434945, 77.95057265855270145 ) ) ;
#9167 = DIRECTION ( 'NONE',  ( -1.402518428993831183E-16, 1.000000000000000000, -3.469446951953617147E-16 ) ) ;
#9168 = DIRECTION ( 'NONE',  ( 1.000000000000000000, 1.402518428993831676E-16, 1.621236893436268400E-16 ) ) ;
#9169 = VECTOR ( 'NONE', #12215, 1000.000000000000000 ) ;
#9170 = ORIENTED_EDGE ( 'NONE', *, *, #9675, .F. ) ;
#9171 = LINE ( 'NONE', #4253, #15317 ) ;
#9172 = VECTOR ( 'NONE', #15220, 1000.000000000000114 ) ;
#9173 = CARTESIAN_POINT ( 'NONE',  ( -6.792737292293178797, 47.86790251333490431, 78.78375056423675460 ) ) ;
#9174 = VERTEX_POINT ( 'NONE', #3690 ) ;
#9175 = CARTESIAN_POINT ( 'NONE',  ( 0.5934291639749685876, 52.36187159818830850, 75.36022115247205022 ) ) ;
#9176 = AXIS2_PLACEMENT_3D ( 'NONE', #2959, #12752, #14556 ) ;
#9177 = ORIENTED_EDGE ( 'NONE', *, *, #5040, .T. ) ;
#9178 = DIRECTION ( 'NONE',  ( -0.000000000000000000, 2.168404344970984413E-15, -1.000000000000000000 ) ) ;
#9179 = CARTESIAN_POINT ( 'NONE',  ( -4.500660556396669065, 42.81632233694663370, 94.32058880294496817 ) ) ;
#9180 =( BOUNDED_CURVE ( )  B_SPLINE_CURVE ( 2, ( #2244, #15229, #12046, #17237, #5957, #1075, #7236, #7665, #9377, #7563, #14143 ),
 .UNSPECIFIED., .F., .T. ) 
 B_SPLINE_CURVE_WITH_KNOTS ( ( 3, 2, 2, 2, 2, 3 ),
 ( 0.2673390146554854296, 0.2812500000000000000, 0.3125000000000000000, 0.3437500000000000000, 0.3750000000000000000, 0.3923390146554854296 ),
 .UNSPECIFIED. ) 
 CURVE ( )  GEOMETRIC_REPRESENTATION_ITEM ( )  RATIONAL_B_SPLINE_CURVE ( ( 0.9623977609649205789, 0.9661148573551011642, 1.000000000000000000, 0.9238795325112867385, 1.000000000000000000, 0.9238795325112867385, 1.000000000000000000, 0.9238795325112867385, 1.000000000000000000, 0.9577646751561855742, 0.9623977609649205789 ) ) 
 REPRESENTATION_ITEM ( '' )  );
#9181 = VERTEX_POINT ( 'NONE', #10211 ) ;
#9182 = CARTESIAN_POINT ( 'NONE',  ( 2.921181103050038530, 49.30691215337508737, 93.50121379782399345 ) ) ;
#9184 = AXIS2_PLACEMENT_3D ( 'NONE', #12740, #16147, #6334 ) ;
#9183 = CARTESIAN_POINT ( 'NONE',  ( -0.9175459788215616364, 52.21929978415766982, 76.23506554152810111 ) ) ;
#9185 = AXIS2_PLACEMENT_3D ( 'NONE', #5453, #784, #16851 ) ;
#9186 = CARTESIAN_POINT ( 'NONE',  ( -4.330063686617302565, 50.77263821455978388, 75.97757385978665923 ) ) ;
#9187 = DIRECTION ( 'NONE',  ( -0.7071067811865506814, 0.7071067811865443531, 0.000000000000000000 ) ) ;
#9188 = FILL_AREA_STYLE_COLOUR ( '', #6010 ) ;
#9189 = CARTESIAN_POINT ( 'NONE',  ( -3.527921555204845738, 37.12740924552473842, 79.39152984579853012 ) ) ;
#9190 = ORIENTED_EDGE ( 'NONE', *, *, #7673, .T. ) ;
#9191 = CARTESIAN_POINT ( 'NONE',  ( 1.456841371642047411, 39.25032235153333460, 92.45433879953097289 ) ) ;
#9192 = ADVANCED_FACE ( 'NONE', ( #6980 ), #13702, .F. ) ;
#9193 = EDGE_LOOP ( 'NONE', ( #18009, #8545, #9634, #453 ) ) ;
#9194 = CARTESIAN_POINT ( 'NONE',  ( 5.230203880350988044, 37.63038499358497546, 75.36022115247205022 ) ) ;
#9195 = LINE ( 'NONE', #12171, #6684 ) ;
#9196 = CARTESIAN_POINT ( 'NONE',  ( -4.524181921268124462, 40.28999182795290324, 94.78933880123798872 ) ) ;
#9197 = VECTOR ( 'NONE', #18416, 1000.000000000000000 ) ;
#9198 = AXIS2_PLACEMENT_3D ( 'NONE', #20492, #12105, #3999 ) ;
#9199 = CARTESIAN_POINT ( 'NONE',  ( 4.394343283833276992, 39.11584570990505938, 95.10183880123797451 ) ) ;
#9200 = DIRECTION ( 'NONE',  ( -1.540237394707283727E-16, -1.793354297423763257E-16, 1.000000000000000000 ) ) ;
#9201 = FACE_OUTER_BOUND ( 'NONE', #9405, .T. ) ;
#9202 = CARTESIAN_POINT ( 'NONE',  ( 5.655950003444441876, 37.76811099897118851, 78.37198585835440667 ) ) ;
#9203 = B_SPLINE_SURFACE_WITH_KNOTS ( 'NONE', 3, 1, ( 
 ( #5479, #3574 ),
 ( #10186, #20156 ),
 ( #13467, #19939 ),
 ( #10079, #5366 ),
 ( #18359, #16561 ),
 ( #8791, #18572 ),
 ( #8689, #7180 ),
 ( #10405, #15394 ),
 ( #15070, #6866 ),
 ( #1982, #8477 ),
 ( #3779, #15281 ),
 ( #15170, #18466 ),
 ( #16669, #701 ),
 ( #586, #3881 ),
 ( #2293, #16973 ) ),
 .UNSPECIFIED., .F., .F., .F.,
 ( 4, 1, 1, 1, 1, 1, 1, 1, 1, 1, 1, 1, 4 ),
 ( 2, 2 ),
 ( 0.000000000000000000, 0.1176523470896303353, 0.2161622001139844318, 0.3003057309359747351, 0.3785980537073788676, 0.4226998745584166772, 0.4746596431302817498, 0.5370400780653459272, 0.6084305140821594238, 0.6909958779695384301, 0.7839813792576545426, 0.8861497511813531958, 0.9999999999999998890 ),
 ( 0.000000000000000000, 1.000000000000000000 ),
 .UNSPECIFIED. ) ;
#9204 = ORIENTED_EDGE ( 'NONE', *, *, #14549, .T. ) ;
#9205 = CARTESIAN_POINT ( 'NONE',  ( 8.214833241226736860, 41.32269513172508368, 76.35929938113996229 ) ) ;
#9206 = VERTEX_POINT ( 'NONE', #606 ) ;
#9207 = DIRECTION ( 'NONE',  ( 0.5941461771851728191, 0.8043570849667734945, 2.357623395011397284E-16 ) ) ;
#9208 = CARTESIAN_POINT ( 'NONE',  ( 6.198496396448986090, 45.68315280215533392, 95.49246380123798872 ) ) ;
#9209 = VECTOR ( 'NONE', #13515, 1000.000000000000000 ) ;
#9210 = CARTESIAN_POINT ( 'NONE',  ( 5.429452001895136881, 51.47777242866884251, 75.37972891991934432 ) ) ;
#9211 = ORIENTED_EDGE ( 'NONE', *, *, #20151, .F. ) ;
#9212 = CARTESIAN_POINT ( 'NONE',  ( -5.154188915835984375, 42.64120994080404614, 94.86746380123797451 ) ) ;
#9213 = CARTESIAN_POINT ( 'NONE',  ( -5.323589340698339001, 50.80079960963960417, 79.37256909934775706 ) ) ;
#9214 = CARTESIAN_POINT ( 'NONE',  ( 2.232254456934871456, 39.46371826755015633, 93.42308879611699979 ) ) ;
#9215 = CARTESIAN_POINT ( 'NONE',  ( 6.114519447167765520, 37.34250893849451813, 78.36972961004526894 ) ) ;
#9216 = CARTESIAN_POINT ( 'NONE',  ( 5.209619950776937181, 50.88551756745181365, 76.17377400622436312 ) ) ;
#9217 = EDGE_CURVE ( 'NONE', #5140, #6553, #13588, .T. ) ;
#9218 = ORIENTED_EDGE ( 'NONE', *, *, #6946, .T. ) ;
#9219 = DIRECTION ( 'NONE',  ( -0.3015081906286224966, 0.9534635866061452747, 1.245503830460468587E-16 ) ) ;
#9220 = CARTESIAN_POINT ( 'NONE',  ( 3.460444912181559474, 49.25145096859824889, 90.64871380123798872 ) ) ;
#9221 = EDGE_CURVE ( 'NONE', #8340, #12307, #7200, .T. ) ;
#9222 = VERTEX_POINT ( 'NONE', #4006 ) ;
#9223 = CARTESIAN_POINT ( 'NONE',  ( -5.005367866107262032, 50.21986932831274686, 79.33799273367436911 ) ) ;
#9224 = PLANE ( 'NONE',  #1366 ) ;
#9225 = CARTESIAN_POINT ( 'NONE',  ( 0.7901638384306272078, 50.30062182352762079, 94.82933879782397923 ) ) ;
#9226 = CARTESIAN_POINT ( 'NONE',  ( -3.799282117832333494, 36.41383735683930212, 77.78682928037112276 ) ) ;
#9227 = CARTESIAN_POINT ( 'NONE',  ( 8.787869161997047485, 41.13152587271654426, 76.34522901481825841 ) ) ;
#9228 = LINE ( 'NONE', #4100, #17082 ) ;
#9229 = EDGE_CURVE ( 'NONE', #15854, #618, #5706, .T. ) ;
#9230 = VERTEX_POINT ( 'NONE', #14219 ) ;
#9231 = CARTESIAN_POINT ( 'NONE',  ( 2.064224670253138605, 52.95475613764697442, 76.07541412571639228 ) ) ;
#9232 = ORIENTED_EDGE ( 'NONE', *, *, #3722, .T. ) ;
#9233 = CARTESIAN_POINT ( 'NONE',  ( 6.591015671753180705, 50.61977213638343187, 75.57514290624801845 ) ) ;
#9234 = CARTESIAN_POINT ( 'NONE',  ( 5.330578599509985693, 37.52924894288483415, 77.75763958275959453 ) ) ;
#9235 = CARTESIAN_POINT ( 'NONE',  ( 2.043125170982144745, 38.48583871533720213, 95.02371380123798872 ) ) ;
#9236 = CARTESIAN_POINT ( 'NONE',  ( 31.07218010054375412, 42.76218137147968434, 70.80574467885102763 ) ) ;
#9237 = ORIENTED_EDGE ( 'NONE', *, *, #14809, .F. ) ;
#9238 = VECTOR ( 'NONE', #843, 1000.000000000000000 ) ;
#9239 = CARTESIAN_POINT ( 'NONE',  ( -4.611439147851055687, 37.01374503923339176, 75.36135576041903050 ) ) ;
#9240 = EDGE_CURVE ( 'NONE', #3158, #2032, #5822, .T. ) ;
#9241 = CARTESIAN_POINT ( 'NONE',  ( -4.898310004515241900, 46.00518860734035087, 92.45433879953095868 ) ) ;
#9242 = ORIENTED_EDGE ( 'NONE', *, *, #19379, .T. ) ;
#9243 = DIRECTION ( 'NONE',  ( 1.779391786395883536E-16, 5.922860397471806844E-17, -1.000000000000000000 ) ) ;
#9244 = EDGE_CURVE ( 'NONE', #445, #4372, #2426, .T. ) ;
#9245 = FACE_OUTER_BOUND ( 'NONE', #2341, .T. ) ;
#9246 = CARTESIAN_POINT ( 'NONE',  ( 4.512269934384615766, 47.81844922806527620, 91.62621379953098710 ) ) ;
#9247 = EDGE_CURVE ( 'NONE', #19774, #1868, #20276, .T. ) ;
#9248 = VERTEX_POINT ( 'NONE', #10527 ) ;
#9249 = CARTESIAN_POINT ( 'NONE',  ( 2.522153740306494196, 49.81903562097208749, 67.21119304902339309 ) ) ;
#9250 = CARTESIAN_POINT ( 'NONE',  ( -7.435811987448031068, 40.12253007576792641, 78.82487260570216847 ) ) ;
#9251 = CARTESIAN_POINT ( 'NONE',  ( 9.539487329945080418, 45.16218137147971845, 95.45352954694192249 ) ) ;
#9252 = CARTESIAN_POINT ( 'NONE',  ( -2.416137431568557314, 39.07291177436112406, 96.11746380123797451 ) ) ;
#9253 = CARTESIAN_POINT ( 'NONE',  ( 31.22215374030650281, 45.56218137147968861, 78.80433879953099563 ) ) ;
#9254 = FACE_OUTER_BOUND ( 'NONE', #4651, .T. ) ;
#9255 = ADVANCED_FACE ( 'NONE', ( #928 ), #13906, .T. ) ;
#9256 = EDGE_CURVE ( 'NONE', #12581, #11222, #7636, .T. ) ;
#9257 = CARTESIAN_POINT ( 'NONE',  ( 1.256812508749381774, 49.74246873332880625, 93.92996380294498238 ) ) ;
#9258 = VECTOR ( 'NONE', #18512, 1000.000000000000000 ) ;
#9259 = CARTESIAN_POINT ( 'NONE',  ( 2.522153740306511072, 50.16218137147969713, 53.15433879953100416 ) ) ;
#9260 = CARTESIAN_POINT ( 'NONE',  ( 8.949918141112842562, 41.61719694332212072, 78.74360054667872078 ) ) ;
#9261 = VECTOR ( 'NONE', #5298, 1000.000000000000000 ) ;
#9262 = LINE ( 'NONE', #10965, #11194 ) ;
#9263 = ORIENTED_EDGE ( 'NONE', *, *, #19610, .T. ) ;
#9264 = CARTESIAN_POINT ( 'NONE',  ( -1.077846259693496345, 47.82824192744436687, 77.55433879953099563 ) ) ;
#9265 = FACE_OUTER_BOUND ( 'NONE', #20854, .T. ) ;
#9266 = CARTESIAN_POINT ( 'NONE',  ( 8.515342467852711650, 40.31474608159486195, 79.26294543469528264 ) ) ;
#9267 = DIRECTION ( 'NONE',  ( 1.000000000000000000, 2.838338907332122006E-16, -0.000000000000000000 ) ) ;
#9268 = VERTEX_POINT ( 'NONE', #10948 ) ;
#9269 = VECTOR ( 'NONE', #12315, 1000.000000000000000 ) ;
#9270 = CARTESIAN_POINT ( 'NONE',  ( 8.641109729321982513, 43.05609659325752858, 78.59572304307680213 ) ) ;
#9272 = EDGE_CURVE ( 'NONE', #3440, #9317, #15833, .T. ) ;
#9271 = CARTESIAN_POINT ( 'NONE',  ( -4.751859364981149803, 37.11746779715601718, 79.54765774203875139 ) ) ;
#9273 = DIRECTION ( 'NONE',  ( -0.5941461771851691553, -0.8043570849667760481, -2.357623395011396791E-16 ) ) ;
#9274 = VECTOR ( 'NONE', #3230, 1000.000000000000000 ) ;
#9275 = CARTESIAN_POINT ( 'NONE',  ( 28.52215374030650352, 44.16218137147969003, 105.5543387995309956 ) ) ;
#9276 = DIRECTION ( 'NONE',  ( -0.6546536707079712025, 0.6546536707079816386, 0.3779644730092298621 ) ) ;
#9277 = CARTESIAN_POINT ( 'NONE',  ( 0.5221537403065006355, 44.16218137147969003, 92.45433879953097289 ) ) ;
#9278 = CARTESIAN_POINT ( 'NONE',  ( 14.52215374030650175, 44.16218137147969003, 105.5543387995309956 ) ) ;
#9279 = ADVANCED_FACE ( 'NONE', ( #10745 ), #17207, .F. ) ;
#9280 = ADVANCED_FACE ( 'NONE', ( #1041 ), #1381, .T. ) ;
#9281 = VERTEX_POINT ( 'NONE', #20808 ) ;
#9282 = CARTESIAN_POINT ( 'NONE',  ( 6.198496396448986090, 45.68315280215533392, 91.58621380123798872 ) ) ;
#9283 = AXIS2_PLACEMENT_3D ( 'NONE', #4195, #3873, #11871 ) ;
#9284 = CARTESIAN_POINT ( 'NONE',  ( -4.630794176838950449, 51.29584566888366481, 79.54703672271651271 ) ) ;
#9286 = ORIENTED_EDGE ( 'NONE', *, *, #20418, .F. ) ;
#9285 = VECTOR ( 'NONE', #5625, 999.9999999999998863 ) ;
#9287 = CARTESIAN_POINT ( 'NONE',  ( 5.873343927958857513, 51.14988734394304970, 77.25083512729199242 ) ) ;
#9288 = EDGE_LOOP ( 'NONE', ( #1538, #1484, #19335, #19115 ) ) ;
#9289 = DIRECTION ( 'NONE',  ( -1.000000000000000000, 0.000000000000000000, 0.000000000000000000 ) ) ;
#9290 = CARTESIAN_POINT ( 'NONE',  ( -5.058133621542618030, 44.89684013992257405, 90.49246380294498238 ) ) ;
#9291 = ORIENTED_EDGE ( 'NONE', *, *, #19459, .T. ) ;
#9292 = PLANE ( 'NONE',  #13021 ) ;
#9293 = CARTESIAN_POINT ( 'NONE',  ( -0.9343110595793820972, 52.97862540336715398, 76.74746709665741662 ) ) ;
#9294 = CARTESIAN_POINT ( 'NONE',  ( -4.244029479098209379, 50.83477438462418974, 75.97198585835440099 ) ) ;
#9295 = FACE_OUTER_BOUND ( 'NONE', #17799, .T. ) ;
#9296 = CARTESIAN_POINT ( 'NONE',  ( 0.7930981759416947385, 52.96401942048080969, 76.04568394904065087 ) ) ;
#9297 = CARTESIAN_POINT ( 'NONE',  ( -3.535132420242974138, 36.21872061582890723, 78.58910375170351870 ) ) ;
#9298 = ORIENTED_EDGE ( 'NONE', *, *, #9915, .T. ) ;
#9299 = DIRECTION ( 'NONE',  ( -0.000000000000000000, 1.000000000000000000, -0.000000000000000000 ) ) ;
#9300 = VECTOR ( 'NONE', #19806, 999.9999999999998863 ) ;
#9301 = CARTESIAN_POINT ( 'NONE',  ( -1.419351766502867429, 49.49642391118513274, 92.25121379782397923 ) ) ;
#9302 = VERTEX_POINT ( 'NONE', #11050 ) ;
#9303 = CARTESIAN_POINT ( 'NONE',  ( 4.394343283833276992, 39.11584570990505938, 95.10183880123797451 ) ) ;
#9304 = EDGE_CURVE ( 'NONE', #18617, #6536, #17522, .T. ) ;
#9305 = CARTESIAN_POINT ( 'NONE',  ( 31.07218010054375412, 42.76218137147968434, 64.80574467885102763 ) ) ;
#9306 = LINE ( 'NONE', #14170, #13888 ) ;
#9307 = CARTESIAN_POINT ( 'NONE',  ( 5.694963103159264683, 37.04270933600420079, 75.97340568087561508 ) ) ;
#9308 = CARTESIAN_POINT ( 'NONE',  ( -5.907462774012221196, 37.97106548486249267, 76.06004113464240390 ) ) ;
#9309 = ORIENTED_EDGE ( 'NONE', *, *, #3228, .F. ) ;
#9310 = CARTESIAN_POINT ( 'NONE',  ( 2.813615989083933844, 36.91585811327294664, 75.45433879953087342 ) ) ;
#9311 =( BOUNDED_CURVE ( )  B_SPLINE_CURVE ( 3, ( #20214, #5434, #8864, #10785 ),
 .UNSPECIFIED., .F., .F. ) 
 B_SPLINE_CURVE_WITH_KNOTS ( ( 4, 4 ),
 ( 4.188790204786388749, 4.300872134317199169 ),
 .UNSPECIFIED. ) 
 CURVE ( )  GEOMETRIC_REPRESENTATION_ITEM ( )  RATIONAL_B_SPLINE_CURVE ( ( 1.000000000000000000, 0.9989534107080366709, 0.9989534107080366709, 1.000000000000000000 ) ) 
 REPRESENTATION_ITEM ( '' )  );
#9312 = EDGE_LOOP ( 'NONE', ( #8094, #2375, #16847, #15378 ) ) ;
#9313 = AXIS2_PLACEMENT_3D ( 'NONE', #16977, #20261, #14778 ) ;
#9314 = CARTESIAN_POINT ( 'NONE',  ( -3.777846259693486974, 36.96218137147968008, 93.55433879953098142 ) ) ;
#9315 = CARTESIAN_POINT ( 'NONE',  ( -0.9988176903691428077, 49.83852402762217082, 94.55496380123798872 ) ) ;
#9316 = CARTESIAN_POINT ( 'NONE',  ( 4.575658464751415799, 52.10843532165534953, 76.08931382966170531 ) ) ;
#9317 = VERTEX_POINT ( 'NONE', #1669 ) ;
#9318 = CARTESIAN_POINT ( 'NONE',  ( -1.348357406114881751, 47.70104341108812918, 85.28382765310961133 ) ) ;
#9319 = ORIENTED_EDGE ( 'NONE', *, *, #20151, .T. ) ;
#9320 = CARTESIAN_POINT ( 'NONE',  ( -4.518589064258795140, 36.94516042271329326, 78.67445481091525039 ) ) ;
#9321 = ADVANCED_FACE ( 'NONE', ( #14432 ), #20384, .F. ) ;
#9322 = CARTESIAN_POINT ( 'NONE',  ( 1.059694531045822563, 38.29779899706197455, 95.05433879953093879 ) ) ;
#9323 = ORIENTED_EDGE ( 'NONE', *, *, #17525, .F. ) ;
#9324 = CARTESIAN_POINT ( 'NONE',  ( -4.500660556396669065, 42.81632233694663370, 92.75808879953098085 ) ) ;
#9325 = CARTESIAN_POINT ( 'NONE',  ( 5.568489401881125289, 48.03437091500646261, 93.07058880123797451 ) ) ;
#9326 = ORIENTED_EDGE ( 'NONE', *, *, #15324, .T. ) ;
#9327 = CARTESIAN_POINT ( 'NONE',  ( 0.5221537403065015237, 44.16218137147968292, 75.45433879953088763 ) ) ;
#9328 = CARTESIAN_POINT ( 'NONE',  ( 5.988021488050563335, 43.25938002633461110, 95.05433879953098142 ) ) ;
#9329 = CARTESIAN_POINT ( 'NONE',  ( -4.812088799398939187, 42.22067586467031930, 92.71996379782397923 ) ) ;
#9330 = CIRCLE ( 'NONE', #16790, 4.200000000000001066 ) ;
#9331 = CARTESIAN_POINT ( 'NONE',  ( 4.199109002476567376, 47.83913663364971569, 93.80036078555450274 ) ) ;
#9332 = FACE_OUTER_BOUND ( 'NONE', #13391, .T. ) ;
#9333 = CARTESIAN_POINT ( 'NONE',  ( -7.211434918694761720, 41.43606403771804025, 78.45489642720582424 ) ) ;
#9334 = VERTEX_POINT ( 'NONE', #12947 ) ;
#9335 = CARTESIAN_POINT ( 'NONE',  ( -7.154059339130676598, 47.04588606493869918, 77.58227997600145898 ) ) ;
#9336 = EDGE_CURVE ( 'NONE', #16327, #15690, #15222, .T. ) ;
#9337 = ORIENTED_EDGE ( 'NONE', *, *, #6382, .T. ) ;
#9338 = LINE ( 'NONE', #20889, #11913 ) ;
#9339 = CARTESIAN_POINT ( 'NONE',  ( 5.769916034762062829, 37.09626795672559041, 77.71701144737939160 ) ) ;
#9340 = CARTESIAN_POINT ( 'NONE',  ( -5.784195910403845176, 44.99242805365518194, 95.88308880123798872 ) ) ;
#9341 = DIRECTION ( 'NONE',  ( 1.334402673828313339E-16, -1.592765810570777996E-32, -1.000000000000000000 ) ) ;
#9342 = ORIENTED_EDGE ( 'NONE', *, *, #15289, .F. ) ;
#9343 = CARTESIAN_POINT ( 'NONE',  ( -4.007890887056452023, 40.01116025973682611, 93.89183879782397923 ) ) ;
#9344 = ORIENTED_EDGE ( 'NONE', *, *, #16125, .F. ) ;
#9345 = CARTESIAN_POINT ( 'NONE',  ( -3.878807879564845962, 37.39741278052461837, 75.39293290059653430 ) ) ;
#9346 = CARTESIAN_POINT ( 'NONE',  ( -5.405803290722375642, 49.82780803385384871, 76.66164947481811964 ) ) ;
#9347 = ORIENTED_EDGE ( 'NONE', *, *, #10271, .T. ) ;
#9348 = CARTESIAN_POINT ( 'NONE',  ( 4.202207491541066098, 51.47027350681489111, 78.92424046551381878 ) ) ;
#9349 = CARTESIAN_POINT ( 'NONE',  ( -6.716320333671362164, 40.30932109133388508, 78.68352653107739059 ) ) ;
#9350 = CARTESIAN_POINT ( 'NONE',  ( 8.389283321988518338, 39.93693882439677623, 76.47636794762235013 ) ) ;
#9351 = ADVANCED_FACE ( 'NONE', ( #11364 ), #17834, .T. ) ;
#9352 = ORIENTED_EDGE ( 'NONE', *, *, #16117, .T. ) ;
#9353 = CARTESIAN_POINT ( 'NONE',  ( 5.987192815050652150, 50.27622337231140648, 75.44981441668713273 ) ) ;
#9354 = CARTESIAN_POINT ( 'NONE',  ( 5.819883890974968388, 51.18937611976139834, 77.96367690144739981 ) ) ;
#9355 = CARTESIAN_POINT ( 'NONE',  ( 6.450247442662826458, 38.49669771550791353, 76.69330938776616335 ) ) ;
#9356 = CARTESIAN_POINT ( 'NONE',  ( 6.828503391016846891, 43.33193468930419101, 92.91433880123798872 ) ) ;
#9357 = CARTESIAN_POINT ( 'NONE',  ( -4.699374957658429608, 51.24684035381270064, 75.36124333316173818 ) ) ;
#9358 = LINE ( 'NONE', #7751, #11300 ) ;
#9359 = CARTESIAN_POINT ( 'NONE',  ( 0.5221537403065118488, 48.16218137147969003, 45.55433879953100273 ) ) ;
#9360 = CARTESIAN_POINT ( 'NONE',  ( -4.677846311233868626, 45.55551708285101142, 92.96487682030837618 ) ) ;
#9361 = ORIENTED_EDGE ( 'NONE', *, *, #14734, .T. ) ;
#9362 = B_SPLINE_CURVE_WITH_KNOTS ( 'NONE', 3,
 ( #16257, #7960, #3367, #14445, #8060, #20913, #14758, #14552, #12849, #4745, #6453 ),
 .UNSPECIFIED., .F., .F.,
 ( 4, 1, 1, 1, 1, 1, 1, 1, 4 ),
 ( 0.000000000000000000, 0.1182921183292337947, 0.2229146666077276573, 0.3191072744444787279, 0.4123240778398947204, 0.5160602913484956256, 0.6446607815519475038, 0.8056994663548258107, 1.000000000000000000 ),
 .UNSPECIFIED. ) ;
#9363 = CARTESIAN_POINT ( 'NONE',  ( 4.539372959821318609, 52.13523796247791608, 76.58963291717793709 ) ) ;
#9364 = CARTESIAN_POINT ( 'NONE',  ( -5.368445182934982185, 36.96218137147968008, 80.55433879953099563 ) ) ;
#9365 = CARTESIAN_POINT ( 'NONE',  ( 5.575778192174150050, 51.36968716628822307, 76.13411024644928204 ) ) ;
#9366 = DIRECTION ( 'NONE',  ( -2.838338907332122006E-16, 1.000000000000000000, 0.000000000000000000 ) ) ;
#9367 = ORIENTED_EDGE ( 'NONE', *, *, #4787, .F. ) ;
#9368 = CARTESIAN_POINT ( 'NONE',  ( -7.594489630341222153, 43.08133907316179290, 78.79856413697085316 ) ) ;
#9369 = FACE_OUTER_BOUND ( 'NONE', #13457, .T. ) ;
#9370 = ORIENTED_EDGE ( 'NONE', *, *, #5694, .F. ) ;
#9371 = CARTESIAN_POINT ( 'NONE',  ( 8.214956227423224178, 41.32302818927274757, 78.56413997391275927 ) ) ;
#9372 = CARTESIAN_POINT ( 'NONE',  ( -4.069601230858992835, 36.61351119651401120, 79.44037905412795908 ) ) ;
#9373 = CARTESIAN_POINT ( 'NONE',  ( 5.076572431691917409, 37.34329067111212197, 77.43080938776617472 ) ) ;
#9374 = DIRECTION ( 'NONE',  ( -0.000000000000000000, -0.000000000000000000, 1.000000000000000000 ) ) ;
#9375 = B_SPLINE_SURFACE_WITH_KNOTS ( 'NONE', 3, 1, ( 
 ( #10200, #11479 ),
 ( #19440, #3370 ),
 ( #1890, #19850 ),
 ( #13278, #19543 ),
 ( #8378, #14972 ),
 ( #19747, #8487 ),
 ( #6877, #5169 ),
 ( #16570, #3581 ),
 ( #391, #13381 ),
 ( #10088, #4959 ),
 ( #3480, #11786 ),
 ( #8603, #18261 ),
 ( #11379, #14760 ),
 ( #1797, #5271 ),
 ( #13068, #8278 ),
 ( #1992, #3681 ),
 ( #16678, #2101 ),
 ( #17849, #15081 ),
 ( #3273, #495 ),
 ( #9779, #1685 ),
 ( #8166, #14653 ),
 ( #14424, #11252 ),
 ( #16033, #19416 ),
 ( #12938, #7941 ),
 ( #7838, #11142 ),
 ( #3042, #19114 ),
 ( #7730, #19005 ) ),
 .UNSPECIFIED., .F., .F., .F.,
 ( 4, 1, 1, 1, 1, 1, 1, 1, 1, 1, 1, 1, 1, 1, 1, 1, 1, 1, 1, 1, 1, 1, 1, 1, 4 ),
 ( 2, 2 ),
 ( 0.000000000000000000, 0.05993306358482522467, 0.1145105083304139432, 0.1639926324650750333, 0.2083799252409545000, 0.2474206522578790979, 0.2813744068707942358, 0.3102651545178817805, 0.3340707221093189849, 0.3764843156245091249, 0.4195869878574357559, 0.4649490021377667981, 0.5131068515344550107, 0.5381792345077858197, 0.5638273912065150384, 0.5896398555221948889, 0.6163062535856453916, 0.6433841197412238921, 0.6712141767968796691, 0.7000136030487154049, 0.7297781433983795418, 0.7919609919944711196, 0.8575419152218471952, 0.9267698348267595643, 1.000000000000000000 ),
 ( 0.000000000000000000, 1.000000000000000000 ),
 .UNSPECIFIED. ) ;
#9376 = CARTESIAN_POINT ( 'NONE',  ( 5.374867109526370257, 50.76497661324683719, 77.94915300234312383 ) ) ;
#9377 = CARTESIAN_POINT ( 'NONE',  ( -1.590937568396969315, 39.63064243629642647, 93.26683879611698558 ) ) ;
#9378 = DIRECTION ( 'NONE',  ( 1.196361017915039239E-16, 0.000000000000000000, -1.000000000000000000 ) ) ;
#9379 = DIRECTION ( 'NONE',  ( -1.779391786395883536E-16, -5.922860397471806844E-17, 1.000000000000000000 ) ) ;
#9380 = CARTESIAN_POINT ( 'NONE',  ( 4.394343283833276992, 39.11584570990505938, 91.35183880123798872 ) ) ;
#9381 = ADVANCED_FACE ( 'NONE', ( #11468 ), #17938, .T. ) ;
#9382 = CARTESIAN_POINT ( 'NONE',  ( -5.261478123908109872, 50.84518201112111058, 79.40394833312912226 ) ) ;
#9383 = EDGE_CURVE ( 'NONE', #10724, #13622, #8759, .T. ) ;
#9384 = CARTESIAN_POINT ( 'NONE',  ( 5.248942363195014948, 50.86274201606274659, 78.77059126715526816 ) ) ;
#9385 = EDGE_LOOP ( 'NONE', ( #18245, #14638, #2397, #6874 ) ) ;
#9386 = DIRECTION ( 'NONE',  ( 1.540237394707284220E-16, 1.793354297423764243E-16, -1.000000000000000000 ) ) ;
#9387 = B_SPLINE_CURVE_WITH_KNOTS ( 'NONE', 3,
 ( #19657, #3594, #13489, #8503, #14988, #10005, #5390, #8712, #1904, #6892, #14772, #5083, #11601, #13396, #18076, #2746, #18704, #7317 ),
 .UNSPECIFIED., .F., .F.,
 ( 4, 2, 2, 2, 2, 2, 2, 2, 4 ),
 ( 0.000000000000000000, 0.0003586288075955534156, 0.0007172576151911068312, 0.001075886422786660138, 0.001434515230382213662, 0.001793144037977766969, 0.001972458441775543948, 0.002151772845573320277, 0.002869030460764344492 ),
 .UNSPECIFIED. ) ;
#9388 = EDGE_CURVE ( 'NONE', #20491, #17689, #17933, .T. ) ;
#9389 = CARTESIAN_POINT ( 'NONE',  ( -2.077846259693550746, 39.65884927180063357, 90.72683880294498238 ) ) ;
#9390 = ORIENTED_EDGE ( 'NONE', *, *, #15208, .F. ) ;
#9391 = CARTESIAN_POINT ( 'NONE',  ( 5.753005855668248181, 51.23877623043087937, 78.93669174070734584 ) ) ;
#9392 = CARTESIAN_POINT ( 'NONE',  ( -0.9278697225093164302, 52.97857461105712673, 76.50701133828320621 ) ) ;
#9393 = CARTESIAN_POINT ( 'NONE',  ( 4.989364768915854675, 51.80284713987553857, 79.39429067157672648 ) ) ;
#9394 = DIRECTION ( 'NONE',  ( -5.626130192357176673E-16, -1.831515347669941892E-30, 1.000000000000000000 ) ) ;
#9395 = PLANE ( 'NONE',  #12145 ) ;
#9396 = CARTESIAN_POINT ( 'NONE',  ( -0.3436364127516083888, 49.62902198444135138, 92.45433879953095868 ) ) ;
#9397 = EDGE_LOOP ( 'NONE', ( #16615, #8608, #17498, #11784 ) ) ;
#9398 = CARTESIAN_POINT ( 'NONE',  ( 2.119851040271390374, 52.81592988514039178, 77.84551527011910821 ) ) ;
#9399 = ORIENTED_EDGE ( 'NONE', *, *, #17785, .F. ) ;
#9400 = CARTESIAN_POINT ( 'NONE',  ( 1.352400422481993658, 50.46853102219002096, 95.57058880123798872 ) ) ;
#9401 = CARTESIAN_POINT ( 'NONE',  ( -3.350035803220276609, 49.20851703305431357, 94.47683880123798872 ) ) ;
#9402 = DIRECTION ( 'NONE',  ( 1.000000000000000000, 0.000000000000000000, 0.000000000000000000 ) ) ;
#9403 = PLANE ( 'NONE',  #5917 ) ;
#9404 = CARTESIAN_POINT ( 'NONE',  ( -5.955289093497882824, 38.00639286050488863, 76.68644156968609593 ) ) ;
#9405 = EDGE_LOOP ( 'NONE', ( #3557, #20714, #15680, #10394 ) ) ;
#9406 = PLANE ( 'NONE',  #15278 ) ;
#9407 = ORIENTED_EDGE ( 'NONE', *, *, #16213, .F. ) ;
#9408 = VECTOR ( 'NONE', #19320, 1000.000000000000000 ) ;
#9409 = CARTESIAN_POINT ( 'NONE',  ( -3.906146384357795043, 51.81365245034167799, 75.48713596493043099 ) ) ;
#9410 = EDGE_CURVE ( 'NONE', #17793, #8117, #9078, .T. ) ;
#9411 = CARTESIAN_POINT ( 'NONE',  ( -4.567115856812060670, 47.10047254335474065, 93.46121380123797451 ) ) ;
#9412 = FACE_OUTER_BOUND ( 'NONE', #5549, .T. ) ;
#9413 = VERTEX_POINT ( 'NONE', #16942 ) ;
#9414 = CARTESIAN_POINT ( 'NONE',  ( -5.181694682358441995, 49.98224533783228907, 79.13778479689705136 ) ) ;
#9415 = CARTESIAN_POINT ( 'NONE',  ( 2.635245049009968810, 48.69372030666295359, 93.89183879611699979 ) ) ;
#9416 = ORIENTED_EDGE ( 'NONE', *, *, #6268, .T. ) ;
#9417 = CARTESIAN_POINT ( 'NONE',  ( 4.753159030984773992, 36.36973062767617648, 75.61597629374708163 ) ) ;
#9418 = CARTESIAN_POINT ( 'NONE',  ( 5.570264759168902735, 51.37375971715457013, 76.17377400622436312 ) ) ;
#9419 = VERTEX_POINT ( 'NONE', #13648 ) ;
#9420 = LINE ( 'NONE', #20876, #19353 ) ;
#9421 = CARTESIAN_POINT ( 'NONE',  ( -4.567115856812060670, 47.10047254335474065, 90.96121380123797451 ) ) ;
#9422 = EDGE_LOOP ( 'NONE', ( #14980, #368, #18355, #4163, #14532, #7474, #3091, #20741 ) ) ;
#9423 = LINE ( 'NONE', #15912, #11114 ) ;
#9424 = FACE_OUTER_BOUND ( 'NONE', #15554, .T. ) ;
#9425 = CARTESIAN_POINT ( 'NONE',  ( -4.622577041588897373, 46.56120873422322859, 93.81371379782397923 ) ) ;
#9426 = AXIS2_PLACEMENT_3D ( 'NONE', #18435, #8760, #12380 ) ;
#9427 = DIRECTION ( 'NONE',  ( -2.267473790562806355E-16, 5.922860397471811774E-17, -1.000000000000000000 ) ) ;
#9428 =( BOUNDED_CURVE ( )  B_SPLINE_CURVE ( 3, ( #17065, #10488, #2063, #7155 ),
 .UNSPECIFIED., .F., .F. ) 
 B_SPLINE_CURVE_WITH_KNOTS ( ( 4, 4 ),
 ( 1.230959417340773854, 1.276280841686759260 ),
 .UNSPECIFIED. ) 
 CURVE ( )  GEOMETRIC_REPRESENTATION_ITEM ( )  RATIONAL_B_SPLINE_CURVE ( ( 1.000000000000000000, 0.9998288380325437430, 0.9998288380325437430, 1.000000000000000000 ) ) 
 REPRESENTATION_ITEM ( '' )  );
#9429 = CARTESIAN_POINT ( 'NONE',  ( 8.862035351310685982, 41.35380664710483245, 75.97281361087948426 ) ) ;
#9430 = CARTESIAN_POINT ( 'NONE',  ( 5.928804517645879457, 51.10892084043006633, 76.16996516156804375 ) ) ;
#9431 = B_SPLINE_CURVE_WITH_KNOTS ( 'NONE', 3,
 ( #17406, #10935, #11245, #3035, #1445, #17718, #11350, #12623, #20588, #6016, #20792, #12516, #7830, #18998 ),
 .UNSPECIFIED., .F., .F.,
 ( 4, 2, 2, 2, 2, 2, 4 ),
 ( 0.000000000000000000, 0.0004302987682907632766, 0.0006454481524361446168, 0.0008605975365815261196, 0.001075746920726907731, 0.001290896304872289017, 0.001721195073163036627 ),
 .UNSPECIFIED. ) ;
#9432 = ORIENTED_EDGE ( 'NONE', *, *, #19002, .T. ) ;
#9433 = CARTESIAN_POINT ( 'NONE',  ( -7.145525873512015735, 47.06850347111571864, 78.12199217155379927 ) ) ;
#9434 = CARTESIAN_POINT ( 'NONE',  ( 5.981342461385748877, 37.24734554037533485, 78.37107466246847309 ) ) ;
#9435 = CARTESIAN_POINT ( 'NONE',  ( -6.753843712027885360, 40.38066566033639759, 75.45433879953087342 ) ) ;
#9436 = VERTEX_POINT ( 'NONE', #11957 ) ;
#9437 = DIRECTION ( 'NONE',  ( 0.5813877811926998485, -0.8136266022444382795, -5.636455622144657394E-17 ) ) ;
#9438 = CARTESIAN_POINT ( 'NONE',  ( 0.5221537403065015237, 44.16218137147968292, 75.45433879953088763 ) ) ;
#9439 = CARTESIAN_POINT ( 'NONE',  ( 6.828503391016846891, 43.33193468930419101, 92.91433880123798872 ) ) ;
#9440 = B_SPLINE_CURVE_WITH_KNOTS ( 'NONE', 3,
 ( #17553, #17245, #2980, #2669, #14472, #1284, #10882, #11187, #20538, #19059, #7672, #12461, #1083, #5866 ),
 .UNSPECIFIED., .F., .F.,
 ( 4, 2, 2, 2, 2, 2, 4 ),
 ( 0.000000000000000000, 0.0001389616711475478018, 0.0002779233422950956036, 0.0003474041778688886678, 0.0004168850134426816778, 0.0004863658490164747420, 0.0005558466845902677519 ),
 .UNSPECIFIED. ) ;
#9441 = CARTESIAN_POINT ( 'NONE',  ( 0.5221537403064990812, 44.16218137147969003, 95.05433879953096721 ) ) ;
#9442 = ORIENTED_EDGE ( 'NONE', *, *, #13144, .T. ) ;
#9443 = ORIENTED_EDGE ( 'NONE', *, *, #9244, .F. ) ;
#9444 = STYLED_ITEM ( 'NONE', ( #20908 ), #11671 ) ;
#9445 = CARTESIAN_POINT ( 'NONE',  ( -3.165374202885676613, 36.87042806242320125, 75.89423958357750166 ) ) ;
#9446 = CARTESIAN_POINT ( 'NONE',  ( 8.355456706376745757, 41.73731273165762445, 78.88551942360874136 ) ) ;
#9447 = CARTESIAN_POINT ( 'NONE',  ( 5.830039445700249345, 50.26785961534839942, 79.48482414599367019 ) ) ;
#9448 = ORIENTED_EDGE ( 'NONE', *, *, #17925, .F. ) ;
#9449 = CARTESIAN_POINT ( 'NONE',  ( -4.480134106163296437, 37.69151641300361177, 77.31947969467269388 ) ) ;
#9450 = CARTESIAN_POINT ( 'NONE',  ( 8.221051890839362386, 41.35279423182788605, 77.39661844205990349 ) ) ;
#9451 = CARTESIAN_POINT ( 'NONE',  ( -3.467962453771611830, 40.50591351489412517, 93.50121379953097289 ) ) ;
#9452 = EDGE_LOOP ( 'NONE', ( #6272, #12630, #2087, #14602 ) ) ;
#9453 = CARTESIAN_POINT ( 'NONE',  ( 5.497743849324331578, 37.64424434608246628, 77.37492703482499223 ) ) ;
#9454 = CARTESIAN_POINT ( 'NONE',  ( -7.835841657577859998, 41.38754952096324047, 79.54638463348854316 ) ) ;
#9455 = CARTESIAN_POINT ( 'NONE',  ( -5.510796958474740492, 38.60848837797752964, 78.53742703482498655 ) ) ;
#9456 = CARTESIAN_POINT ( 'NONE',  ( 2.043125170982144745, 38.48583871533720213, 93.92996380123798872 ) ) ;
#9457 = EDGE_CURVE ( 'NONE', #1329, #4901, #13850, .T. ) ;
#9458 = VECTOR ( 'NONE', #13916, 1000.000000000000000 ) ;
#9459 =( NAMED_UNIT ( * ) PLANE_ANGLE_UNIT ( ) SI_UNIT ( $, .RADIAN. ) );
#9460 = CARTESIAN_POINT ( 'NONE',  ( 5.308657174530695855, 50.64216575474389970, 75.36022115247205022 ) ) ;
#9461 = VECTOR ( 'NONE', #4435, 1000.000000000000114 ) ;
#9462 = CARTESIAN_POINT ( 'NONE',  ( -1.477846259693495146, 50.16218137147969713, 82.55433879953099563 ) ) ;
#9463 = DIRECTION ( 'NONE',  ( 0.3165065846431827645, 0.9485903129789529098, 0.000000000000000000 ) ) ;
#9464 = CARTESIAN_POINT ( 'NONE',  ( -0.9429997834273105006, 52.21747844655818227, 77.93056416558285093 ) ) ;
#9465 = ORIENTED_EDGE ( 'NONE', *, *, #15478, .T. ) ;
#9466 = CARTESIAN_POINT ( 'NONE',  ( -4.267481014617145796, 37.50633945324470631, 75.98838203353618326 ) ) ;
#9467 = CARTESIAN_POINT ( 'NONE',  ( 0.5221537403065020788, 52.36218137147968577, 52.53721119516358584 ) ) ;
#9468 = CARTESIAN_POINT ( 'NONE',  ( 8.392124750090893315, 39.94545476467643397, 78.58253683706189463 ) ) ;
#9469 = CARTESIAN_POINT ( 'NONE',  ( -4.524181921268124462, 40.28999182795290324, 91.19558880123797451 ) ) ;
#9470 = VECTOR ( 'NONE', #9167, 1000.000000000000000 ) ;
#9471 = EDGE_LOOP ( 'NONE', ( #19625, #12028, #6951, #10602 ) ) ;
#9472 = ORIENTED_EDGE ( 'NONE', *, *, #8700, .T. ) ;
#9473 = CARTESIAN_POINT ( 'NONE',  ( 8.318328750355229673, 41.62059619433301094, 75.36022115247205022 ) ) ;
#9474 = CARTESIAN_POINT ( 'NONE',  ( -4.473072018670158911, 36.91153881467540998, 79.53329352641277694 ) ) ;
#9475 = CARTESIAN_POINT ( 'NONE',  ( 5.427780505986065762, 36.85179043424346190, 76.70433879953087342 ) ) ;
#9476 = CARTESIAN_POINT ( 'NONE',  ( 31.07218010054375412, 36.96218137147968008, 37.55574467885101342 ) ) ;
#9477 = CARTESIAN_POINT ( 'NONE',  ( 2.122153740306512937, 47.82824192744436687, 53.55433879953100273 ) ) ;
#9478 = ADVANCED_FACE ( 'NONE', ( #18434, #20120 ), #13751, .T. ) ;
#9479 = CARTESIAN_POINT ( 'NONE',  ( 6.680635945739894055, 50.55357325011429026, 77.60602934391619101 ) ) ;
#9480 = DIRECTION ( 'NONE',  ( -1.000000000000000000, 0.000000000000000000, 0.000000000000000000 ) ) ;
#9481 = CARTESIAN_POINT ( 'NONE',  ( 1.514255888186003762, 51.36218137147968577, 87.21440135111343750 ) ) ;
#9482 = B_SPLINE_CURVE_WITH_KNOTS ( 'NONE', 3,
 ( #1956, #12174, #10273, #4180, #8986, #16749, #13760, #4071, #8558, #10706, #676, #2381, #7045, #10598, #3860, #15368, #5664, #785, #7265 ),
 .UNSPECIFIED., .F., .F.,
 ( 4, 1, 1, 1, 1, 1, 1, 1, 1, 1, 1, 1, 1, 1, 1, 1, 4 ),
 ( 0.000000000000000000, 0.06302581646095750667, 0.1222495429959427476, 0.1789669701231155763, 0.2332877456213924006, 0.2860909212508800925, 0.3384954837963008445, 0.3911857795644178570, 0.4453574251251987137, 0.5015394511440722791, 0.5602660668541803446, 0.6223358252984214634, 0.6886061413240012197, 0.7590929558684775813, 0.8342439359547982880, 0.9143471077142913961, 1.000000000000000000 ),
 .UNSPECIFIED. ) ;
#9483 = VECTOR ( 'NONE', #16940, 1000.000000000000227 ) ;
#9484 = CARTESIAN_POINT ( 'NONE',  ( 0.5221537403065048544, 44.16218137147969713, 82.55433879953099563 ) ) ;
#9485 = EDGE_CURVE ( 'NONE', #3115, #4005, #3954, .T. ) ;
#9486 = CARTESIAN_POINT ( 'NONE',  ( 2.337612517491833852, 49.93701999136722947, 72.45432679953087529 ) ) ;
#9487 = CARTESIAN_POINT ( 'NONE',  ( -5.927888611570137911, 47.57933715648534445, 78.32492703482499508 ) ) ;
#9488 = EDGE_CURVE ( 'NONE', #8267, #10926, #15142, .T. ) ;
#9489 = ORIENTED_EDGE ( 'NONE', *, *, #18857, .F. ) ;
#9490 = FACE_OUTER_BOUND ( 'NONE', #15693, .T. ) ;
#9491 = CARTESIAN_POINT ( 'NONE',  ( -0.2125050281363792815, 38.58189400963055959, 92.05496380294498238 ) ) ;
#9492 = ORIENTED_EDGE ( 'NONE', *, *, #16017, .T. ) ;
#9493 = CARTESIAN_POINT ( 'NONE',  ( 4.432284427945813121, 36.14044538431356557, 77.43080938776617472 ) ) ;
#9494 = AXIS2_PLACEMENT_3D ( 'NONE', #12654, #6562, #11687 ) ;
#9495 = CARTESIAN_POINT ( 'NONE',  ( -0.7807185704487904498, 52.97741427014419457, 75.89928829349869943 ) ) ;
#9496 = CARTESIAN_POINT ( 'NONE',  ( 5.706854332355044690, 51.27286650160559134, 79.54768974400036541 ) ) ;
#9497 = CARTESIAN_POINT ( 'NONE',  ( -2.917199766949190476, 51.60602765227618960, 78.10580938776615767 ) ) ;
#9498 = CARTESIAN_POINT ( 'NONE',  ( -0.9947171538446211159, 49.52734785157042552, 92.45433879953102974 ) ) ;
#9499 = EDGE_CURVE ( 'NONE', #4554, #15837, #16738, .T. ) ;
#9500 = ORIENTED_EDGE ( 'NONE', *, *, #5545, .F. ) ;
#9501 = EDGE_CURVE ( 'NONE', #8403, #492, #19965, .T. ) ;
#9502 = PLANE ( 'NONE',  #5786 ) ;
#9503 = ORIENTED_EDGE ( 'NONE', *, *, #1418, .F. ) ;
#9504 = EDGE_CURVE ( 'NONE', #3488, #10737, #8975, .T. ) ;
#9505 = DIRECTION ( 'NONE',  ( -5.626130192357176673E-16, -1.831515347669941892E-30, 1.000000000000000000 ) ) ;
#9506 = CARTESIAN_POINT ( 'NONE',  ( -6.851854717395867489, 47.75120794669041402, 78.80861213953217259 ) ) ;
#9507 = CARTESIAN_POINT ( 'NONE',  ( 1.110644313093400504, 52.20952139108884893, 76.77233108029956554 ) ) ;
#9508 = CARTESIAN_POINT ( 'NONE',  ( 2.232254456934871012, 39.46371826755015633, 94.67308879611699979 ) ) ;
#9509 = CARTESIAN_POINT ( 'NONE',  ( 8.496652696354052736, 46.09822506120844565, 76.54154894328375747 ) ) ;
#9510 = ADVANCED_FACE ( 'NONE', ( #18540 ), #18643, .F. ) ;
#9511 = AXIS2_PLACEMENT_3D ( 'NONE', #19486, #17794, #3818 ) ;
#9512 = ORIENTED_EDGE ( 'NONE', *, *, #15237, .F. ) ;
#9513 = CARTESIAN_POINT ( 'NONE',  ( 4.582010541884842247, 52.10374329815417127, 78.30859729819620441 ) ) ;
#9514 = ORIENTED_EDGE ( 'NONE', *, *, #13272, .F. ) ;
#9515 = AXIS2_PLACEMENT_3D ( 'NONE', #15476, #2275, #13664 ) ;
#9516 = PLANE ( 'NONE',  #20708 ) ;
#9517 = VECTOR ( 'NONE', #6895, 1000.000000000000000 ) ;
#9518 = CARTESIAN_POINT ( 'NONE',  ( 6.198496396448986090, 45.68315280215533392, 94.24246380123798872 ) ) ;
#9519 = CARTESIAN_POINT ( 'NONE',  ( -8.192078482032011166, 42.93655631659661509, 72.45433879953085921 ) ) ;
#9520 = ORIENTED_EDGE ( 'NONE', *, *, #4663, .F. ) ;
#9521 = CARTESIAN_POINT ( 'NONE',  ( -5.376400592477268425, 49.84311562309974164, 78.65111229433956908 ) ) ;
#9522 = DIRECTION ( 'NONE',  ( 0.000000000000000000, 0.000000000000000000, -1.000000000000000000 ) ) ;
#9523 = CARTESIAN_POINT ( 'NONE',  ( -4.178795553179217137, 37.44880458579923044, 78.81995494622690046 ) ) ;
#9524 = CARTESIAN_POINT ( 'NONE',  ( 5.575778192174150050, 51.36968716628822307, 76.13411024644928204 ) ) ;
#9525 = DIRECTION ( 'NONE',  ( 0.003131479924976700649, -0.009902722955645586189, -0.9999460635011987453 ) ) ;
#9526 = ORIENTED_EDGE ( 'NONE', *, *, #13270, .F. ) ;
#9527 = VECTOR ( 'NONE', #11996, 1000.000000000000114 ) ;
#9528 = CARTESIAN_POINT ( 'NONE',  ( -4.956235989166514422, 43.70076514643270116, 92.55433879953098142 ) ) ;
#9529 = VECTOR ( 'NONE', #14180, 1000.000000000000000 ) ;
#9530 = FACE_OUTER_BOUND ( 'NONE', #12477, .T. ) ;
#9531 = ORIENTED_EDGE ( 'NONE', *, *, #18748, .T. ) ;
#9532 = CARTESIAN_POINT ( 'NONE',  ( 4.359773538758245692, 47.36728266200564263, 95.05433879953096721 ) ) ;
#9533 = CARTESIAN_POINT ( 'NONE',  ( 5.505261640620147112, 46.12417297501537661, 95.05433879953093879 ) ) ;
#9534 = EDGE_CURVE ( 'NONE', #16835, #6239, #18808, .T. ) ;
#9535 = CIRCLE ( 'NONE', #8510, 6.000000000000002665 ) ;
#9536 = CARTESIAN_POINT ( 'NONE',  ( 0.7926596301127065702, 52.95803722965069227, 78.84197725022382031 ) ) ;
#9537 = CARTESIAN_POINT ( 'NONE',  ( 2.921181103050039418, 49.30691215337508737, 92.25121379782397923 ) ) ;
#9538 = AXIS2_PLACEMENT_3D ( 'NONE', #17186, #3981, #12191 ) ;
#9539 = CARTESIAN_POINT ( 'NONE',  ( 0.5221537403065114047, 44.16218137147969713, 45.55433879953100273 ) ) ;
#9540 = EDGE_CURVE ( 'NONE', #12039, #496, #7360, .T. ) ;
#9541 = LINE ( 'NONE', #18027, #11558 ) ;
#9542 = CARTESIAN_POINT ( 'NONE',  ( 5.933960187751527116, 51.10511255460609448, 76.21496574784163158 ) ) ;
#9543 = ORIENTED_EDGE ( 'NONE', *, *, #20540, .F. ) ;
#9544 = CARTESIAN_POINT ( 'NONE',  ( 2.069840415553682700, 52.20187471152334524, 78.81257284323012868 ) ) ;
#9545 = VECTOR ( 'NONE', #3500, 1000.000000000000000 ) ;
#9546 = ORIENTED_EDGE ( 'NONE', *, *, #5944, .T. ) ;
#9547 = CARTESIAN_POINT ( 'NONE',  ( -5.917125461193805336, 40.64525615903904310, 76.16022115247204738 ) ) ;
#9548 = EDGE_CURVE ( 'NONE', #19487, #12818, #2577, .T. ) ;
#9549 = CARTESIAN_POINT ( 'NONE',  ( 5.485216391323153751, 37.63974744726360910, 77.55803991379978868 ) ) ;
#9550 = CARTESIAN_POINT ( 'NONE',  ( 9.318068138769051600, 42.72056584129816059, 78.97126489842982267 ) ) ;
#9551 = B_SPLINE_SURFACE_WITH_KNOTS ( 'NONE', 3, 1, ( 
 ( #14403, #6002 ),
 ( #17591, #1325 ),
 ( #4600, #7810 ),
 ( #19093, #19394 ),
 ( #1221, #6303 ),
 ( #12913, #4810 ),
 ( #6406, #12607 ),
 ( #2817, #3018 ),
 ( #9524, #1533 ),
 ( #9418, #9216 ),
 ( #6100, #1122 ),
 ( #4503, #15906 ),
 ( #7710, #16008 ),
 ( #3127, #12804 ),
 ( #2710, #7915 ) ),
 .UNSPECIFIED., .F., .F., .F.,
 ( 4, 1, 1, 1, 1, 1, 1, 1, 1, 1, 1, 1, 4 ),
 ( 2, 2 ),
 ( 0.000000000000000000, 0.1100843045400305420, 0.2037028897711227471, 0.2865965782701816456, 0.3664837514983516065, 0.4113922274074651164, 0.4651658430714658010, 0.5281943374952151604, 0.6014928947756199573, 0.6850328536222562992, 0.7789954854465236389, 0.8848457782734755472, 1.000000000000000000 ),
 ( 0.000000000000000000, 1.000000000000000000 ),
 .UNSPECIFIED. ) ;
#9552 = ORIENTED_EDGE ( 'NONE', *, *, #21006, .F. ) ;
#9553 = DIRECTION ( 'NONE',  ( 0.9999689119394085113, -0.007885122365275831768, 1.526048693634352652E-16 ) ) ;
#9554 = ORIENTED_EDGE ( 'NONE', *, *, #4824, .F. ) ;
#9555 = AXIS2_PLACEMENT_3D ( 'NONE', #1388, #13089, #4984 ) ;
#9556 = LINE ( 'NONE', #14215, #19957 ) ;
#9557 = CARTESIAN_POINT ( 'NONE',  ( -4.664487479516255419, 37.05292970491732518, 75.97486526700035370 ) ) ;
#9558 = LINE ( 'NONE', #19011, #20139 ) ;
#9559 = ORIENTED_EDGE ( 'NONE', *, *, #8694, .F. ) ;
#9560 = CARTESIAN_POINT ( 'NONE',  ( -4.399781695603910414, 37.63216332411592191, 77.30667006270941499 ) ) ;
#9561 = CARTESIAN_POINT ( 'NONE',  ( 8.274195582100176694, 41.51206924590946556, 77.52203278780699236 ) ) ;
#9562 = CARTESIAN_POINT ( 'NONE',  ( -1.876873622437038369, 39.01745058958429269, 91.46996379782397923 ) ) ;
#9563 = ORIENTED_EDGE ( 'NONE', *, *, #15958, .T. ) ;
#9564 = CARTESIAN_POINT ( 'NONE',  ( -7.775939518413485629, 41.23271989474202570, 78.69802408570997443 ) ) ;
#9565 =( NAMED_UNIT ( * ) PLANE_ANGLE_UNIT ( ) SI_UNIT ( $, .RADIAN. ) );
#9566 = CARTESIAN_POINT ( 'NONE',  ( -5.488960544945736153, 38.58484428221787965, 78.87558661569313756 ) ) ;
#9567 = CARTESIAN_POINT ( 'NONE',  ( -3.350035803220276609, 49.20851703305431357, 95.72683880123798872 ) ) ;
#9568 = CARTESIAN_POINT ( 'NONE',  ( -5.818890812078571173, 50.44687531233557110, 76.28720437108826502 ) ) ;
#9569 = CARTESIAN_POINT ( 'NONE',  ( -8.080465354403330025, 46.01554175503538602, 72.45433879953085921 ) ) ;
#9570 = PLANE ( 'NONE',  #16632 ) ;
#9571 = CARTESIAN_POINT ( 'NONE',  ( -0.8447986058118214237, 52.97914482513772327, 78.90127229107831397 ) ) ;
#9572 = CARTESIAN_POINT ( 'NONE',  ( 25.63948732994508362, 43.16218137147969003, 76.90433879953101837 ) ) ;
#9573 = CARTESIAN_POINT ( 'NONE',  ( 8.643936145691096584, 43.06456754242027074, 76.74257409364852833 ) ) ;
#9574 = DIRECTION ( 'NONE',  ( 3.620524460287508833E-17, -1.000000000000000000, -7.183611964723545059E-17 ) ) ;
#9575 = DIRECTION ( 'NONE',  ( -1.779391786395883536E-16, -5.922860397471806844E-17, 1.000000000000000000 ) ) ;
#9576 = VECTOR ( 'NONE', #6638, 1000.000000000000114 ) ;
#9577 = VERTEX_POINT ( 'NONE', #4478 ) ;
#9578 = ORIENTED_EDGE ( 'NONE', *, *, #741, .F. ) ;
#9579 = CARTESIAN_POINT ( 'NONE',  ( 9.332226353535185481, 42.76299890913265500, 76.00948821603452643 ) ) ;
#9580 = CARTESIAN_POINT ( 'NONE',  ( -7.677846259693480668, 36.96218137147968008, 95.05433879953098142 ) ) ;
#9581 = CARTESIAN_POINT ( 'NONE',  ( -4.886362818588793289, 37.21682008020638222, 78.74088963820604192 ) ) ;
#9582 = CARTESIAN_POINT ( 'NONE',  ( 3.122153740306552905, 48.66551347115873227, 91.03933879953099506 ) ) ;
#9583 = DIRECTION ( 'NONE',  ( 1.000000000000000000, 0.000000000000000000, 0.000000000000000000 ) ) ;
#9584 = DIRECTION ( 'NONE',  ( -1.540237394707284220E-16, -1.793354297423764243E-16, 1.000000000000000000 ) ) ;
#9585 = CARTESIAN_POINT ( 'NONE',  ( -3.057592722523234219, 36.78482279269636734, 76.43665125469834720 ) ) ;
#9586 = VECTOR ( 'NONE', #2202, 999.9999999999998863 ) ;
#9587 = B_SPLINE_CURVE_WITH_KNOTS ( 'NONE', 3,
 ( #1737, #18501, #16305, #19582, #17891, #8719, #10332, #15204, #10440, #3913, #3313, #7098, #16804, #14704 ),
 .UNSPECIFIED., .F., .F.,
 ( 4, 2, 2, 2, 2, 2, 4 ),
 ( 0.000000000000000000, 6.877694998478215750E-05, 0.0001375538999695643150, 0.0002063308499543464725, 0.0002751077999391286300, 0.0004126616999087005886, 0.0005502155998782725472 ),
 .UNSPECIFIED. ) ;
#9588 = DIRECTION ( 'NONE',  ( 1.000000000000000000, 0.000000000000000000, 0.000000000000000000 ) ) ;
#9589 = DIRECTION ( 'NONE',  ( 0.000000000000000000, 1.000000000000000000, 0.000000000000000000 ) ) ;
#9590 = CARTESIAN_POINT ( 'NONE',  ( 0.5221537403065105165, 44.16218137147969713, 50.55433879953100273 ) ) ;
#9591 = ORIENTED_EDGE ( 'NONE', *, *, #15209, .F. ) ;
#9592 = LINE ( 'NONE', #1712, #3084 ) ;
#9593 = DIRECTION ( 'NONE',  ( 3.893792155548169402E-16, 7.183611964723547524E-17, -1.000000000000000000 ) ) ;
#9594 = ADVANCED_FACE ( 'NONE', ( #9295 ), #5881, .F. ) ;
#9595 = CARTESIAN_POINT ( 'NONE',  ( 5.518796429342951448, 36.91682708076865538, 78.21801395346943764 ) ) ;
#9596 = ORIENTED_EDGE ( 'NONE', *, *, #2570, .F. ) ;
#9597 = CIRCLE ( 'NONE', #7208, 4.999999999999997335 ) ;
#9598 = LINE ( 'NONE', #17557, #8856 ) ;
#9599 = VECTOR ( 'NONE', #5854, 1000.000000000000114 ) ;
#9600 = CARTESIAN_POINT ( 'NONE',  ( 8.887668352622405621, 41.43063037816333605, 75.36022115247205022 ) ) ;
#9601 = ORIENTED_EDGE ( 'NONE', *, *, #11333, .F. ) ;
#9602 = CARTESIAN_POINT ( 'NONE',  ( 5.833066520072705430, 37.14139298144173296, 75.36337631951366234 ) ) ;
#9603 = CARTESIAN_POINT ( 'NONE',  ( 1.652727357819364418, 35.35299279957455099, 76.16022115247204738 ) ) ;
#9604 = CARTESIAN_POINT ( 'NONE',  ( 5.777481493531589685, 38.02144953885154877, 78.35997004935869370 ) ) ;
#9605 = CARTESIAN_POINT ( 'NONE',  ( 0.5753960310588919214, 52.96573608190006865, 75.97198585835440099 ) ) ;
#9606 = DIRECTION ( 'NONE',  ( 0.5813877811927011807, -0.8136266022444372803, -5.636455622144619183E-17 ) ) ;
#9607 = ORIENTED_EDGE ( 'NONE', *, *, #10649, .F. ) ;
#9608 = CARTESIAN_POINT ( 'NONE',  ( 0.3869120917952217908, 35.96329670974014192, 72.45433879953085921 ) ) ;
#9609 = EDGE_CURVE ( 'NONE', #12054, #10195, #14067, .T. ) ;
#9610 = ORIENTED_EDGE ( 'NONE', *, *, #16773, .T. ) ;
#9611 = CARTESIAN_POINT ( 'NONE',  ( -4.567115856812060670, 47.10047254335474065, 95.80496380123798872 ) ) ;
#9612 = CARTESIAN_POINT ( 'NONE',  ( -4.524181921268124462, 40.28999182795290324, 93.53933880123797451 ) ) ;
#9613 = DIRECTION ( 'NONE',  ( 0.3165065846431829311, 0.9485903129789527988, 2.188653791613874255E-16 ) ) ;
#9614 = CARTESIAN_POINT ( 'NONE',  ( 30.92220646078100188, 42.76218137147968434, 62.80715055817104542 ) ) ;
#9615 = CARTESIAN_POINT ( 'NONE',  ( -7.923612069094863486, 41.67164428332228709, 78.89026057757155286 ) ) ;
#9616 = AXIS2_PLACEMENT_3D ( 'NONE', #17001, #4326, #5612 ) ;
#9617 = ADVANCED_FACE ( 'NONE', ( #11197 ), #4265, .F. ) ;
#9618 = ORIENTED_EDGE ( 'NONE', *, *, #17946, .F. ) ;
#9619 = CARTESIAN_POINT ( 'NONE',  ( 0.5221537403065042993, 44.16218137147969713, 85.55433879953100984 ) ) ;
#9620 = EDGE_CURVE ( 'NONE', #6883, #6753, #3952, .T. ) ;
#9621 = ORIENTED_EDGE ( 'NONE', *, *, #17009, .F. ) ;
#9622 = CARTESIAN_POINT ( 'NONE',  ( 6.450247442662827346, 38.49669771550791353, 72.45433879953087342 ) ) ;
#9623 = CARTESIAN_POINT ( 'NONE',  ( -0.07555581626192756084, 50.25084051303456079, 77.06567965797611919 ) ) ;
#9624 = CARTESIAN_POINT ( 'NONE',  ( 4.732847133705871734, 51.99232638384451377, 75.72008365543779007 ) ) ;
#9625 = ORIENTED_EDGE ( 'NONE', *, *, #4775, .T. ) ;
#9626 = CARTESIAN_POINT ( 'NONE',  ( -5.403135505393695581, 49.82401183315728588, 78.21416447440572028 ) ) ;
#9627 = CARTESIAN_POINT ( 'NONE',  ( 1.403788643848838724, 39.16218137147968292, 93.38983168766081633 ) ) ;
#9628 = AXIS2_PLACEMENT_3D ( 'NONE', #10691, #7680, #2791 ) ;
#9629 = CARTESIAN_POINT ( 'NONE',  ( 4.695664425361702143, 36.32864708750979332, 75.66510065906194882 ) ) ;
#9630 = CARTESIAN_POINT ( 'NONE',  ( -0.8451447117293342526, 38.43386779256927355, 95.05433879953092458 ) ) ;
#9631 = EDGE_CURVE ( 'NONE', #18045, #3176, #1198, .T. ) ;
#9632 = ADVANCED_FACE ( 'NONE', ( #12379 ), #2680, .F. ) ;
#9633 = FACE_OUTER_BOUND ( 'NONE', #16446, .T. ) ;
#9634 = ORIENTED_EDGE ( 'NONE', *, *, #14201, .T. ) ;
#9635 = DIRECTION ( 'NONE',  ( 0.9485903129789529098, -0.3165065846431826535, 8.934458285744997376E-17 ) ) ;
#9636 = B_SPLINE_CURVE_WITH_KNOTS ( 'NONE', 3,
 ( #14212, #1142, #2838, #2734, #2936, #7630, #19307, #4427, #10940, #14111, #1558, #9656, #19206, #16138, #6324, #4622, #15827, #1238 ),
 .UNSPECIFIED., .F., .F.,
 ( 4, 2, 2, 2, 2, 2, 2, 2, 4 ),
 ( 0.000000000000000000, 0.0006084283796061584065, 0.0009126425694092466087, 0.001216856759212335028, 0.001521070949015423121, 0.001825285138818511432, 0.001977392233720055587, 0.002129499328621599959, 0.002433713518424688270 ),
 .UNSPECIFIED. ) ;
#9637 = CARTESIAN_POINT ( 'NONE',  ( 3.357643116058062649, 37.76218137147968434, 92.03489701350649455 ) ) ;
#9638 = VERTEX_POINT ( 'NONE', #6180 ) ;
#9639 = CARTESIAN_POINT ( 'NONE',  ( 4.145197572768899441, 51.51238443731228500, 78.30859729819620441 ) ) ;
#9640 = CARTESIAN_POINT ( 'NONE',  ( 5.309255083855641821, 37.50457964663987553, 75.97198585835440099 ) ) ;
#9641 = CARTESIAN_POINT ( 'NONE',  ( 0.5221537403065181771, 44.16218137147969003, 56.15433879953099705 ) ) ;
#9642 = CARTESIAN_POINT ( 'NONE',  ( -5.838428831739582492, 50.43291415881836315, 76.76022115247205591 ) ) ;
#9643 = CARTESIAN_POINT ( 'NONE',  ( -1.419351766502868317, 49.49642391118513274, 93.65746379782397923 ) ) ;
#9644 = CARTESIAN_POINT ( 'NONE',  ( 0.7901638384306293172, 50.30062182352762079, 90.92308879782397923 ) ) ;
#9645 = DIRECTION ( 'NONE',  ( -1.540237394707283727E-16, -1.793354297423763257E-16, 1.000000000000000000 ) ) ;
#9646 = VECTOR ( 'NONE', #7897, 1000.000000000000114 ) ;
#9647 = CARTESIAN_POINT ( 'NONE',  ( 5.913630530257057316, 51.12012925366870064, 76.09715583564816654 ) ) ;
#9648 = VERTEX_POINT ( 'NONE', #20746 ) ;
#9649 = CARTESIAN_POINT ( 'NONE',  ( -7.150130606013386014, 47.05633550303845425, 78.03747806989589719 ) ) ;
#9650 = EDGE_CURVE ( 'NONE', #11138, #8922, #14145, .T. ) ;
#9651 = ORIENTED_EDGE ( 'NONE', *, *, #8462, .F. ) ;
#9652 = CARTESIAN_POINT ( 'NONE',  ( 25.63948732994507651, 45.16218137147968292, 74.70433879953100131 ) ) ;
#9653 = EDGE_CURVE ( 'NONE', #9713, #11872, #14160, .T. ) ;
#9654 = CARTESIAN_POINT ( 'NONE',  ( 28.43948732994508077, 43.16218137147969003, 76.90433879953101837 ) ) ;
#9655 = CARTESIAN_POINT ( 'NONE',  ( 8.908783915644443496, 41.49391506008672792, 75.36120592425527320 ) ) ;
#9656 = CARTESIAN_POINT ( 'NONE',  ( -2.964841284551051892, 51.58385076907617162, 76.14610479913682184 ) ) ;
#9657 = VERTEX_POINT ( 'NONE', #9497 ) ;
#9658 = CARTESIAN_POINT ( 'NONE',  ( 5.647726803872021861, 51.31654162509386907, 77.98642840401727483 ) ) ;
#9659 = ORIENTED_EDGE ( 'NONE', *, *, #19651, .T. ) ;
#9660 = CARTESIAN_POINT ( 'NONE',  ( 0.8455950101471348956, 52.35579997042385259, 77.76169174070734869 ) ) ;
#9661 = CARTESIAN_POINT ( 'NONE',  ( -4.522047388140567392, 36.94771494725497973, 76.29203488853940485 ) ) ;
#9662 = ADVANCED_FACE ( 'NONE', ( #18955 ), #10792, .T. ) ;
#9663 = CARTESIAN_POINT ( 'NONE',  ( -3.943187491250720544, 40.73580453397070755, 95.33621379953099506 ) ) ;
#9664 = VERTEX_POINT ( 'NONE', #4576 ) ;
#9665 = CARTESIAN_POINT ( 'NONE',  ( -4.717136037229297862, 37.86658019246193163, 77.33565342272370913 ) ) ;
#9666 = CARTESIAN_POINT ( 'NONE',  ( 8.211514564676907213, 41.32421026028232092, 77.18134264024645574 ) ) ;
#9667 = CARTESIAN_POINT ( 'NONE',  ( 5.052198367669454626, 48.31320248322254685, 92.01683879782399345 ) ) ;
#9668 = ADVANCED_FACE ( 'NONE', ( #10999 ), #2990, .F. ) ;
#9669 = AXIS2_PLACEMENT_3D ( 'NONE', #6313, #3143, #16538 ) ;
#9670 = ORIENTED_EDGE ( 'NONE', *, *, #18444, .T. ) ;
#9671 = CARTESIAN_POINT ( 'NONE',  ( -4.649709362898930998, 51.28232956945436882, 75.97399450257033493 ) ) ;
#9672 = LINE ( 'NONE', #14753, #15557 ) ;
#9673 = DIRECTION ( 'NONE',  ( -1.111814006898795283E-16, 5.922860397471810542E-17, -1.000000000000000000 ) ) ;
#9674 = CARTESIAN_POINT ( 'NONE',  ( -0.3080929418689875576, 37.85583172076933778, 94.94558880123797451 ) ) ;
#9675 = EDGE_CURVE ( 'NONE', #19686, #12584, #2894, .T. ) ;
#9676 = CARTESIAN_POINT ( 'NONE',  ( 5.772314152670717569, 37.86287365998423127, 78.36882016909345339 ) ) ;
#9677 = DIRECTION ( 'NONE',  ( 1.000000000000000000, 0.000000000000000000, 0.000000000000000000 ) ) ;
#9678 = CARTESIAN_POINT ( 'NONE',  ( 0.7150189969462155126, 52.34218787202741652, 76.81551440955847454 ) ) ;
#9679 = CARTESIAN_POINT ( 'NONE',  ( 5.230203880350988044, 37.63038499358497546, 75.36022115247205022 ) ) ;
#9680 = CARTESIAN_POINT ( 'NONE',  ( -0.4905242218931977205, 52.21391051046797571, 79.30111418114536548 ) ) ;
#9681 = VERTEX_POINT ( 'NONE', #17567 ) ;
#9682 = DIRECTION ( 'NONE',  ( 0.5941461771851782592, 0.8043570849667694977, 2.357623395011398763E-16 ) ) ;
#9683 = FACE_OUTER_BOUND ( 'NONE', #8144, .T. ) ;
#9684 = CARTESIAN_POINT ( 'NONE',  ( 0.8455950101471351177, 52.35579997042385259, 76.48963291717792856 ) ) ;
#9685 = CARTESIAN_POINT ( 'NONE',  ( 6.778550821858020825, 50.48124747537763568, 77.88538524077617353 ) ) ;
#9686 = VERTEX_POINT ( 'NONE', #15984 ) ;
#9687 = EDGE_CURVE ( 'NONE', #4876, #15492, #3101, .T. ) ;
#9688 = EDGE_LOOP ( 'NONE', ( #15560, #3560, #14575, #2235, #10797, #3257 ) ) ;
#9689 =( BOUNDED_CURVE ( )  B_SPLINE_CURVE ( 3, ( #20517, #18824, #945, #9151 ),
 .UNSPECIFIED., .F., .F. ) 
 B_SPLINE_CURVE_WITH_KNOTS ( ( 4, 4 ),
 ( 1.748195931235267064, 1.749653718118951762 ),
 .UNSPECIFIED. ) 
 CURVE ( )  GEOMETRIC_REPRESENTATION_ITEM ( )  RATIONAL_B_SPLINE_CURVE ( ( 1.000000000000000000, 0.9999998229047912801, 0.9999998229047912801, 1.000000000000000000 ) ) 
 REPRESENTATION_ITEM ( '' )  );
#9690 = DIRECTION ( 'NONE',  ( 0.3165065846431827645, 0.9485903129789529098, 0.000000000000000000 ) ) ;
#9691 = SURFACE_SIDE_STYLE ('',( #19761 ) ) ;
#9692 = DIRECTION ( 'NONE',  ( -1.540237394707284220E-16, -1.793354297423764243E-16, 1.000000000000000000 ) ) ;
#9693 = CARTESIAN_POINT ( 'NONE',  ( 4.903749685900197441, 51.09391985211853893, 79.50087752586969714 ) ) ;
#9694 = LINE ( 'NONE', #20928, #2159 ) ;
#9695 = CARTESIAN_POINT ( 'NONE',  ( 5.599231707071657738, 51.35236299959863970, 78.30875056423674607 ) ) ;
#9696 = FACE_OUTER_BOUND ( 'NONE', #19518, .T. ) ;
#9697 = CARTESIAN_POINT ( 'NONE',  ( 9.277577006266444215, 42.59921134847828483, 77.86785210695053649 ) ) ;
#9698 = CARTESIAN_POINT ( 'NONE',  ( 31.07218010054375412, 45.56218137147968861, 70.80574467885102763 ) ) ;
#9699 = EDGE_LOOP ( 'NONE', ( #12431, #13799, #3631 ) ) ;
#9700 = CARTESIAN_POINT ( 'NONE',  ( -5.210464978622037613, 37.45622129019157143, 79.52089765539699329 ) ) ;
#9701 = PLANE ( 'NONE',  #2090 ) ;
#9702 = CARTESIAN_POINT ( 'NONE',  ( 5.282313327535892000, 50.83908068768521815, 78.88513556223540490 ) ) ;
#9703 = CARTESIAN_POINT ( 'NONE',  ( 8.869748494521283888, 41.37692342661967615, 77.52492703482499792 ) ) ;
#9704 = CARTESIAN_POINT ( 'NONE',  ( 8.774405178022840701, 41.09117345860662596, 75.37437276336991943 ) ) ;
#9705 = ORIENTED_EDGE ( 'NONE', *, *, #10808, .T. ) ;
#9706 = CARTESIAN_POINT ( 'NONE',  ( 6.136807603568960268, 37.35843523903731977, 75.40772603260481333 ) ) ;
#9707 = CARTESIAN_POINT ( 'NONE',  ( 4.578029447411149810, 52.10668397227361481, 78.50413411530853125 ) ) ;
#9708 = CARTESIAN_POINT ( 'NONE',  ( 6.830172062167755520, 37.85388809545894873, 77.80469260682309596 ) ) ;
#9709 = CARTESIAN_POINT ( 'NONE',  ( 4.102496745554329749, 51.53925067467379506, 76.40131969043289928 ) ) ;
#9710 = CARTESIAN_POINT ( 'NONE',  ( -0.9199438314403606265, 52.23437776363726215, 75.45433879953088763 ) ) ;
#9711 = ORIENTED_EDGE ( 'NONE', *, *, #17552, .F. ) ;
#9712 = CARTESIAN_POINT ( 'NONE',  ( 8.345083808671303061, 41.72452575800834751, 76.03029119948048731 ) ) ;
#9713 = VERTEX_POINT ( 'NONE', #6073 ) ;
#9714 = CARTESIAN_POINT ( 'NONE',  ( 4.454347278305088587, 39.79502279609036464, 90.11785590924256439 ) ) ;
#9715 = ADVANCED_FACE ( 'NONE', ( #12578 ), #12424, .T. ) ;
#9716 = CARTESIAN_POINT ( 'NONE',  ( 0.4436773671319499401, 52.36183473419609413, 75.99664209308157581 ) ) ;
#9717 = CARTESIAN_POINT ( 'NONE',  ( -3.096195867026992232, 36.80851087063928873, 78.43912781517941823 ) ) ;
#9718 = DIRECTION ( 'NONE',  ( -1.540237394707284220E-16, -1.793354297423764243E-16, 1.000000000000000000 ) ) ;
#9719 = B_SPLINE_SURFACE_WITH_KNOTS ( 'NONE', 3, 1, ( 
 ( #1301, #6184 ),
 ( #12688, #15987 ),
 ( #19167, #12383 ),
 ( #17571, #18858 ),
 ( #19576, #1832 ),
 ( #1923, #9712 ),
 ( #4788, #319 ),
 ( #19371, #9813 ),
 ( #14896, #20952 ),
 ( #8318, #3306 ),
 ( #16297, #19683 ),
 ( #16508, #11729 ),
 ( #17783, #11311 ),
 ( #6812, #5108 ),
 ( #11626, #3210 ) ),
 .UNSPECIFIED., .F., .F., .F.,
 ( 4, 1, 1, 1, 1, 1, 1, 1, 1, 1, 1, 1, 4 ),
 ( 2, 2 ),
 ( 0.000000000000000000, 0.07577303389073718198, 0.1558117613168219784, 0.2417361372947465226, 0.3357870204060591224, 0.3882587240527491379, 0.4455552461494497463, 0.5113167710153618817, 0.5866953322903324386, 0.6731791507778834838, 0.7705825181721650541, 0.8794626622360116608, 1.000000000000000000 ),
 ( 0.000000000000000000, 1.000000000000000000 ),
 .UNSPECIFIED. ) ;
#9720 = ORIENTED_EDGE ( 'NONE', *, *, #8442, .T. ) ;
#9721 = CARTESIAN_POINT ( 'NONE',  ( -4.517374237173715557, 36.94426307888177519, 76.44623874561141008 ) ) ;
#9722 = EDGE_CURVE ( 'NONE', #5725, #3856, #19367, .T. ) ;
#9723 = VERTEX_POINT ( 'NONE', #14586 ) ;
#9724 = FACE_OUTER_BOUND ( 'NONE', #4415, .T. ) ;
#9725 = CARTESIAN_POINT ( 'NONE',  ( 28.43948732994508077, 36.35905713404685713, 76.90433879953101837 ) ) ;
#9726 = CARTESIAN_POINT ( 'NONE',  ( -2.416137431568557314, 39.07291177436112406, 96.11746380123797451 ) ) ;
#9727 = ORIENTED_EDGE ( 'NONE', *, *, #18945, .T. ) ;
#9728 = CARTESIAN_POINT ( 'NONE',  ( -5.811565481342516826, 50.45210972548208161, 78.65111229433956908 ) ) ;
#9729 = CARTESIAN_POINT ( 'NONE',  ( 0.3869120917952217908, 35.96329670974014192, 72.45433879953085921 ) ) ;
#9730 = CARTESIAN_POINT ( 'NONE',  ( 5.294808925291379254, 46.52673310323378075, 92.55433879953103826 ) ) ;
#9731 = DIRECTION ( 'NONE',  ( -0.3165065846431827645, -0.9485903129789529098, 0.000000000000000000 ) ) ;
#9732 = CARTESIAN_POINT ( 'NONE',  ( 4.199109002476567376, 47.83913663364971569, 83.28180655319408743 ) ) ;
#9733 = EDGE_LOOP ( 'NONE', ( #1766, #20635, #2790, #19124, #7944 ) ) ;
#9734 = CARTESIAN_POINT ( 'NONE',  ( -1.579458713458412822, 38.67424504376464967, 92.55433879953098142 ) ) ;
#9735 = DIRECTION ( 'NONE',  ( -0.9999542261909885044, -0.009567942452870459302, -1.557325602890304767E-16 ) ) ;
#9736 = ORIENTED_EDGE ( 'NONE', *, *, #11100, .F. ) ;
#9737 = CARTESIAN_POINT ( 'NONE',  ( -1.069770211495338019, 49.34613612695786600, 95.05433879953095300 ) ) ;
#9738 = PLANE ( 'NONE',  #18941 ) ;
#9739 = SHAPE_REPRESENTATION ( 'Number Dial Wheels', ( #18366 ), #19057 ) ;
#9740 = CARTESIAN_POINT ( 'NONE',  ( -5.644616003178662744, 50.57140571016744701, 75.79002994479621691 ) ) ;
#9741 = CARTESIAN_POINT ( 'NONE',  ( 5.928963754087451576, 43.92611494815086814, 94.90746379611699979 ) ) ;
#9742 = DIRECTION ( 'NONE',  ( -1.084202172485505420E-16, -1.000000000000000000, 0.000000000000000000 ) ) ;
#9743 = CARTESIAN_POINT ( 'NONE',  ( 0.6404851603139647409, 52.36132752672286017, 79.54845644658969661 ) ) ;
#9744 = VECTOR ( 'NONE', #1399, 1000.000000000000000 ) ;
#9745 = CARTESIAN_POINT ( 'NONE',  ( 5.579255781724441476, 50.61248246897039138, 76.38301527011910252 ) ) ;
#9746 = EDGE_LOOP ( 'NONE', ( #8360, #8440, #17024, #6833 ) ) ;
#9747 = CARTESIAN_POINT ( 'NONE',  ( 1.756236358059617642, 52.20434759476808040, 79.26556901187228732 ) ) ;
#9748 = VERTEX_POINT ( 'NONE', #16406 ) ;
#9749 = CARTESIAN_POINT ( 'NONE',  ( 31.22215374030650281, 42.76218137147968434, 78.80433879953099563 ) ) ;
#9750 = EDGE_CURVE ( 'NONE', #4844, #20845, #19786, .T. ) ;
#9751 = LINE ( 'NONE', #3562, #6500 ) ;
#9752 = CARTESIAN_POINT ( 'NONE',  ( 9.279665234200917823, 42.60546990007262025, 79.15097751326614173 ) ) ;
#9753 = VERTEX_POINT ( 'NONE', #17879 ) ;
#9754 = CARTESIAN_POINT ( 'NONE',  ( 6.828503391016846891, 43.33193468930419101, 94.16433880123797451 ) ) ;
#9755 = CARTESIAN_POINT ( 'NONE',  ( -5.394504046100737860, 38.52817003188538081, 75.85972562479176418 ) ) ;
#9756 = ORIENTED_EDGE ( 'NONE', *, *, #17392, .F. ) ;
#9757 = CARTESIAN_POINT ( 'NONE',  ( 31.07218010054375412, 42.76218137147968434, 69.40574467885102194 ) ) ;
#9758 = CARTESIAN_POINT ( 'NONE',  ( 27.63948732994508717, 45.16218137147969003, 74.70433879953098710 ) ) ;
#9759 = CARTESIAN_POINT ( 'NONE',  ( -0.8237052942265477018, 49.18499566818285018, 96.19558879953099506 ) ) ;
#9760 = ORIENTED_EDGE ( 'NONE', *, *, #15601, .F. ) ;
#9761 = CARTESIAN_POINT ( 'NONE',  ( 5.389492195292208798, 36.82443100924615464, 78.79551527011911105 ) ) ;
#9762 = CARTESIAN_POINT ( 'NONE',  ( -4.620149427167481448, 37.79494009046823777, 77.90250793075740887 ) ) ;
#9763 = CARTESIAN_POINT ( 'NONE',  ( 3.722707913086011011, 40.32076848204647490, 95.05409729707558597 ) ) ;
#9764 = AXIS2_PLACEMENT_3D ( 'NONE', #12977, #6474, #11394 ) ;
#9765 = ORIENTED_EDGE ( 'NONE', *, *, #5329, .F. ) ;
#9766 = CARTESIAN_POINT ( 'NONE',  ( 9.353817388681445522, 42.82770861117572281, 77.06316232894263862 ) ) ;
#9767 = CARTESIAN_POINT ( 'NONE',  ( 10.77494014480653561, 42.96218137147968008, 65.80574467885102763 ) ) ;
#9768 = LINE ( 'NONE', #8270, #14255 ) ;
#9769 = CARTESIAN_POINT ( 'NONE',  ( 3.460444912181559474, 49.25145096859824889, 94.24246380123798872 ) ) ;
#9770 = ADVANCED_FACE ( 'NONE', ( #6488 ), #12995, .T. ) ;
#9771 = B_SPLINE_CURVE_WITH_KNOTS ( 'NONE', 3,
 ( #20519, #7546, #5843, #20193, #12346, #4234, #18508, #3921, #18827, #17225 ),
 .UNSPECIFIED., .F., .F.,
 ( 4, 2, 2, 2, 4 ),
 ( 0.000000000000000000, 0.0003230938241351131719, 0.0004038672801688700112, 0.0004846407362026268506, 0.0006461876482701230193 ),
 .UNSPECIFIED. ) ;
#9772 = UNCERTAINTY_MEASURE_WITH_UNIT (LENGTH_MEASURE( 1.000000000000000082E-05 ), #15646, 'distance_accuracy_value', 'NONE');
#9773 = EDGE_CURVE ( 'NONE', #8610, #17907, #2599, .T. ) ;
#9774 = CARTESIAN_POINT ( 'NONE',  ( 6.244022549736605754, 38.28825185105232265, 78.16399671769941904 ) ) ;
#9775 = DIRECTION ( 'NONE',  ( 1.779391786395883536E-16, 5.922860397471806844E-17, -1.000000000000000000 ) ) ;
#9776 = EDGE_CURVE ( 'NONE', #19886, #11899, #14629, .T. ) ;
#9777 = CARTESIAN_POINT ( 'NONE',  ( -5.478128554961354091, 38.57320898139802523, 72.45433879953085921 ) ) ;
#9778 = EDGE_CURVE ( 'NONE', #15408, #16784, #19711, .T. ) ;
#9779 = CARTESIAN_POINT ( 'NONE',  ( 8.579956030688345336, 40.50839702842124268, 79.37958223971880045 ) ) ;
#9780 = VERTEX_POINT ( 'NONE', #3828 ) ;
#9781 = DIRECTION ( 'NONE',  ( 1.000000000000000000, -4.930380657631323784E-32, 3.893792155548169402E-16 ) ) ;
#9782 = LINE ( 'NONE', #3484, #7543 ) ;
#9783 = DIRECTION ( 'NONE',  ( -1.000000000000000000, 1.110223024625156540E-16, -1.779391786395883043E-16 ) ) ;
#9784 = CARTESIAN_POINT ( 'NONE',  ( 2.522153740306510628, 47.62628298661744708, 53.15433879953100416 ) ) ;
#9785 = EDGE_CURVE ( 'NONE', #15919, #2938, #4633, .T. ) ;
#9786 = ORIENTED_EDGE ( 'NONE', *, *, #8070, .T. ) ;
#9787 = VECTOR ( 'NONE', #15521, 1000.000000000000000 ) ;
#9788 = CARTESIAN_POINT ( 'NONE',  ( 6.634437729966897734, 50.58769801112816111, 77.73730439759678745 ) ) ;
#9789 = CARTESIAN_POINT ( 'NONE',  ( 4.614533305268312624, 51.26839818186464726, 79.40329896012910638 ) ) ;
#9790 = CARTESIAN_POINT ( 'NONE',  ( 2.259191861956057146, 47.76843358786783966, 69.41730067788145675 ) ) ;
#9791 = DIRECTION ( 'NONE',  ( 0.3165065846431826535, 0.9485903129789529098, 2.188653791613874008E-16 ) ) ;
#9792 = VECTOR ( 'NONE', #13287, 1000.000000000000000 ) ;
#9793 = CARTESIAN_POINT ( 'NONE',  ( 9.353817388681445522, 42.82770861117572281, 77.06316232894263862 ) ) ;
#9794 = CARTESIAN_POINT ( 'NONE',  ( -4.477846259693498254, 37.66218137147969713, 53.35433879953099989 ) ) ;
#9795 = CARTESIAN_POINT ( 'NONE',  ( 6.519002636616433755, 49.74813231759035403, 76.51259071708746262 ) ) ;
#9796 = CARTESIAN_POINT ( 'NONE',  ( 2.043125170982144745, 38.48583871533720213, 92.52371380123798872 ) ) ;
#9797 = ORIENTED_EDGE ( 'NONE', *, *, #555, .F. ) ;
#9798 = ADVANCED_FACE ( 'NONE', ( #18409 ), #13944, .T. ) ;
#9799 = LINE ( 'NONE', #16075, #16679 ) ;
#9800 = AXIS2_PLACEMENT_3D ( 'NONE', #17454, #20730, #17547 ) ;
#9801 = FACE_OUTER_BOUND ( 'NONE', #14399, .T. ) ;
#9802 = PLANE ( 'NONE',  #6486 ) ;
#9803 = DIRECTION ( 'NONE',  ( 0.3014921695764776199, -0.9534129230078944861, 0.01030873055283977775 ) ) ;
#9804 = CARTESIAN_POINT ( 'NONE',  ( 9.341681937738675501, 42.79133789484158967, 77.50995918449682165 ) ) ;
#9805 = ORIENTED_EDGE ( 'NONE', *, *, #13480, .F. ) ;
#9806 = ORIENTED_EDGE ( 'NONE', *, *, #1429, .F. ) ;
#9807 = CARTESIAN_POINT ( 'NONE',  ( 0.3848670358072697195, 52.20902977889265628, 75.36353278631986541 ) ) ;
#9808 = CARTESIAN_POINT ( 'NONE',  ( -0.5863195729081820406, 39.16218137147969003, 94.55865272277780775 ) ) ;
#9809 = CARTESIAN_POINT ( 'NONE',  ( 5.953729262864296601, 38.14738974197400978, 78.31663032931759005 ) ) ;
#9810 = CARTESIAN_POINT ( 'NONE',  ( 4.391355930538122010, 51.39239564774072022, 75.64582075504121406 ) ) ;
#9811 = CARTESIAN_POINT ( 'NONE',  ( 5.024485149279870555, 46.57157721280005092, 92.45433879953095868 ) ) ;
#9812 = ORIENTED_EDGE ( 'NONE', *, *, #19274, .T. ) ;
#9813 = CARTESIAN_POINT ( 'NONE',  ( 8.359590704656968185, 41.76800384557771650, 76.08336210994360727 ) ) ;
#9814 = AXIS2_PLACEMENT_3D ( 'NONE', #18782, #13878, #20360 ) ;
#9815 = ORIENTED_EDGE ( 'NONE', *, *, #810, .F. ) ;
#9816 = CARTESIAN_POINT ( 'NONE',  ( -4.524181921268124462, 40.28999182795290324, 91.03933880123798872 ) ) ;
#9817 = LINE ( 'NONE', #12789, #9149 ) ;
#9818 = CARTESIAN_POINT ( 'NONE',  ( 2.522153740306506631, 50.16218137147969713, 77.15433879953100416 ) ) ;
#9819 = CARTESIAN_POINT ( 'NONE',  ( 5.385255718775495026, 47.76702405936703855, 75.45433879953087342 ) ) ;
#9820 = B_SPLINE_CURVE_WITH_KNOTS ( 'NONE', 3,
 ( #8254, #16032, #14319, #12728, #19621, #19521, #4935, #17823, #20891, #5042, #3252, #1453, #20994, #17611, #11141, #9752, #14633, #16235, #9550, #14740, #18036, #60, #7940, #11561, #17927, #14423, #6323 ),
 .UNSPECIFIED., .F., .F.,
 ( 4, 1, 1, 1, 1, 1, 1, 1, 1, 1, 1, 1, 1, 1, 1, 1, 1, 1, 1, 1, 1, 1, 1, 1, 4 ),
 ( 0.000000000000000000, 0.06037445285962812075, 0.1180910611743953287, 0.1732658017268006723, 0.2259310541736886668, 0.2758310469819637567, 0.3235430165773793276, 0.3690552752481174870, 0.4126046436208182233, 0.4542408720228611196, 0.4938267050212239995, 0.5316899362873784840, 0.5681969051958857264, 0.6035856803598054210, 0.6378784996589128564, 0.6713567270158068423, 0.7043713979572046036, 0.7376082755227613141, 0.7714571943499641815, 0.8061103333465380327, 0.8420729482554840661, 0.8794516251380997129, 0.9177737848194706949, 0.9579350591099196066, 1.000000000000000000 ),
 .UNSPECIFIED. ) ;
#9821 = CARTESIAN_POINT ( 'NONE',  ( 8.619779459752459516, 42.86892843748081816, 79.10813152944312776 ) ) ;
#9822 = ORIENTED_EDGE ( 'NONE', *, *, #831, .T. ) ;
#9823 = AXIS2_PLACEMENT_3D ( 'NONE', #15691, #14177, #15998 ) ;
#9824 = ORIENTED_EDGE ( 'NONE', *, *, #17457, .T. ) ;
#9825 = CARTESIAN_POINT ( 'NONE',  ( -7.723289445447552914, 47.23670041943413622, 77.69607208529100717 ) ) ;
#9826 = CARTESIAN_POINT ( 'NONE',  ( 2.580190882731760560, 49.45805475339454205, 94.54925044102853349 ) ) ;
#9827 = CARTESIAN_POINT ( 'NONE',  ( -0.3080929418689875576, 37.85583172076933778, 93.69558880123800293 ) ) ;
#9828 = EDGE_LOOP ( 'NONE', ( #11972, #12572, #172, #14626 ) ) ;
#9829 = EDGE_CURVE ( 'NONE', #5214, #18140, #11376, .T. ) ;
#9830 = CARTESIAN_POINT ( 'NONE',  ( -5.403263942874336756, 49.82392005643602317, 78.10580938776615767 ) ) ;
#9831 = DIRECTION ( 'NONE',  ( 0.9467234622824005630, -0.007465262426704777701, -0.3219611091745780973 ) ) ;
#9832 = CARTESIAN_POINT ( 'NONE',  ( 5.918312273062399598, 44.84149841250357582, 92.55433879953093879 ) ) ;
#9833 = CARTESIAN_POINT ( 'NONE',  ( -1.348357406114871315, 47.70104341108813628, 61.28382765310961844 ) ) ;
#9834 = DIRECTION ( 'NONE',  ( 1.239088197126290817E-16, 1.000000000000000000, 0.000000000000000000 ) ) ;
#9835 = VERTEX_POINT ( 'NONE', #20621 ) ;
#9836 = DIRECTION ( 'NONE',  ( 1.402518428993831676E-16, -1.000000000000000000, 0.000000000000000000 ) ) ;
#9837 = CARTESIAN_POINT ( 'NONE',  ( 0.8448994723799378992, 52.35218080436352039, 78.59044740879555491 ) ) ;
#9838 = ORIENTED_EDGE ( 'NONE', *, *, #2197, .F. ) ;
#9839 = CARTESIAN_POINT ( 'NONE',  ( 3.802468188742213151, 48.04124512683031156, 95.05433879953092458 ) ) ;
#9840 = CARTESIAN_POINT ( 'NONE',  ( -7.674646407923283675, 40.87962920872410422, 76.96732277425439861 ) ) ;
#9841 = VECTOR ( 'NONE', #19877, 1000.000000000000000 ) ;
#9842 = CARTESIAN_POINT ( 'NONE',  ( 0.5221537403065019678, 44.16218137147968292, 72.45433879953087342 ) ) ;
#9843 = CARTESIAN_POINT ( 'NONE',  ( -4.009385194876760927, 46.27527268018315709, 91.70433879611698558 ) ) ;
#9844 = CARTESIAN_POINT ( 'NONE',  ( 2.921181103050039418, 49.30691215337508737, 92.09496379782399345 ) ) ;
#9845 = FACE_OUTER_BOUND ( 'NONE', #14013, .T. ) ;
#9846 = CARTESIAN_POINT ( 'NONE',  ( -7.611372734017124664, 43.12018948500615778, 72.45433879953085921 ) ) ;
#9847 = VECTOR ( 'NONE', #11973, 1000.000000000000000 ) ;
#9848 = CARTESIAN_POINT ( 'NONE',  ( 5.756838674491786101, 51.23594508156129734, 75.97260389846793771 ) ) ;
#9849 = EDGE_LOOP ( 'NONE', ( #4390, #20760, #10558, #3414 ) ) ;
#9850 = CARTESIAN_POINT ( 'NONE',  ( -7.308127660158699967, 41.72770130593617210, 76.16022115247204738 ) ) ;
#9851 = CARTESIAN_POINT ( 'NONE',  ( 6.691294758883309157, 37.75465145915448062, 78.79551527011911105 ) ) ;
#9852 = AXIS2_PLACEMENT_3D ( 'NONE', #16024, #9645, #16126 ) ;
#9853 = B_SPLINE_CURVE_WITH_KNOTS ( 'NONE', 3,
 ( #8169, #83, #14656, #6564, #8280, #19644, #6666, #3483, #14863, #13171, #5496, #598, #2104, #7079, #10311, #8605 ),
 .UNSPECIFIED., .F., .F.,
 ( 4, 2, 2, 2, 2, 2, 2, 4 ),
 ( 0.000000000000000000, 0.0006122100410275824493, 0.0009183150615413739450, 0.001224420082055165115, 0.001377472592312054900, 0.001530525102568944468, 0.001836630123082723604, 0.002448840164110273852 ),
 .UNSPECIFIED. ) ;
#9854 = VERTEX_POINT ( 'NONE', #19240 ) ;
#9855 = LINE ( 'NONE', #16341, #8506 ) ;
#9856 = EDGE_CURVE ( 'NONE', #13175, #18406, #10767, .T. ) ;
#9857 = CARTESIAN_POINT ( 'NONE',  ( 5.241460166982748525, 50.86801069014953924, 78.30875056423674607 ) ) ;
#9858 = CARTESIAN_POINT ( 'NONE',  ( 8.177787109632054907, 41.66748930940789108, 75.36022115247205022 ) ) ;
#9859 = VECTOR ( 'NONE', #6867, 1000.000000000000114 ) ;
#9860 = ORIENTED_EDGE ( 'NONE', *, *, #13374, .F. ) ;
#9861 = VECTOR ( 'NONE', #12625, 1000.000000000000000 ) ;
#9862 = CARTESIAN_POINT ( 'NONE',  ( 23.63948732994508006, 43.16218137147968292, 76.90433879953101837 ) ) ;
#9863 = CARTESIAN_POINT ( 'NONE',  ( -5.943920255163966715, 37.99799515759236357, 76.35020017089209432 ) ) ;
#9864 = EDGE_LOOP ( 'NONE', ( #3095, #4914, #12374, #15346 ) ) ;
#9865 = LINE ( 'NONE', #11771, #20314 ) ;
#9866 = CARTESIAN_POINT ( 'NONE',  ( 30.92220646078100188, 45.56218137147968861, 62.80715055817104542 ) ) ;
#9867 = CARTESIAN_POINT ( 'NONE',  ( 1.256812508749381774, 49.74246873332880625, 94.86746379953099506 ) ) ;
#9868 = ORIENTED_EDGE ( 'NONE', *, *, #3381, .F. ) ;
#9869 = CARTESIAN_POINT ( 'NONE',  ( -5.160557796315995205, 37.41935686500602287, 77.33669174070733732 ) ) ;
#9870 = CARTESIAN_POINT ( 'NONE',  ( -1.477846259693494257, 49.16218137147969003, 74.55433879953100984 ) ) ;
#9871 = CARTESIAN_POINT ( 'NONE',  ( -4.884656273474450749, 44.39824779480852612, 93.34496379953097289 ) ) ;
#9872 = VECTOR ( 'NONE', #697, 1000.000000000000000 ) ;
#9873 = ORIENTED_EDGE ( 'NONE', *, *, #13956, .F. ) ;
#9874 = CARTESIAN_POINT ( 'NONE',  ( -0.8071739151948670310, 40.17810205696807913, 82.45433879953087342 ) ) ;
#9875 = CARTESIAN_POINT ( 'NONE',  ( 1.652727357819364418, 35.35299279957455099, 76.86610350541323555 ) ) ;
#9876 = CARTESIAN_POINT ( 'NONE',  ( 1.490046680165512782, 52.91022367065997400, 75.48600500139500014 ) ) ;
#9877 = CARTESIAN_POINT ( 'NONE',  ( -2.416137431568557314, 39.07291177436112406, 93.61746380123797451 ) ) ;
#9878 = DIRECTION ( 'NONE',  ( 0.000000000000000000, 0.000000000000000000, 1.000000000000000000 ) ) ;
#9879 = ADVANCED_FACE ( 'NONE', ( #9160 ), #12552, .T. ) ;
#9880 = VECTOR ( 'NONE', #16721, 1000.000000000000114 ) ;
#9881 = CARTESIAN_POINT ( 'NONE',  ( 8.648170029844118645, 43.06315486489794608, 78.41904468188381827 ) ) ;
#9882 = AXIS2_PLACEMENT_3D ( 'NONE', #10993, #7777, #14058 ) ;
#9883 = CARTESIAN_POINT ( 'NONE',  ( 0.8277711449680080769, 52.34129877990315549, 76.79008513575435302 ) ) ;
#9884 = CARTESIAN_POINT ( 'NONE',  ( 4.943220423779688844, 37.42531712265408572, 75.37835156746757548 ) ) ;
#9885 = PLANE ( 'NONE',  #20346 ) ;
#9886 =( GEOMETRIC_REPRESENTATION_CONTEXT ( 3 ) GLOBAL_UNCERTAINTY_ASSIGNED_CONTEXT ( ( #10250 ) ) GLOBAL_UNIT_ASSIGNED_CONTEXT ( ( #10286, #6751, #11669 ) ) REPRESENTATION_CONTEXT ( 'NONE', 'WORKASPACE' ) );
#9887 = ORIENTED_EDGE ( 'NONE', *, *, #9488, .F. ) ;
#9888 = CARTESIAN_POINT ( 'NONE',  ( -4.159067576658533660, 37.42968809036762678, 76.29677174223795078 ) ) ;
#9889 = FACE_OUTER_BOUND ( 'NONE', #2049, .T. ) ;
#9890 = CARTESIAN_POINT ( 'NONE',  ( 11.22215374030650281, 42.96218137147968008, 66.20574467885104752 ) ) ;
#9891 = CARTESIAN_POINT ( 'NONE',  ( 6.466516115726876457, 49.79771993804390462, 78.20944795639196911 ) ) ;
#9892 = EDGE_CURVE ( 'NONE', #20138, #13218, #15834, .T. ) ;
#9893 = EDGE_CURVE ( 'NONE', #10515, #13636, #4970, .T. ) ;
#9894 = ORIENTED_EDGE ( 'NONE', *, *, #7, .T. ) ;
#9895 = CARTESIAN_POINT ( 'NONE',  ( 5.406592671645608306, 50.74154221849293833, 78.93606911575150775 ) ) ;
#9896 =( GEOMETRIC_REPRESENTATION_CONTEXT ( 3 ) GLOBAL_UNCERTAINTY_ASSIGNED_CONTEXT ( ( #21012 ) ) GLOBAL_UNIT_ASSIGNED_CONTEXT ( ( #1255, #9459, #1574 ) ) REPRESENTATION_CONTEXT ( 'NONE', 'WORKASPACE' ) );
#9897 = ORIENTED_EDGE ( 'NONE', *, *, #7938, .F. ) ;
#9898 = ADVANCED_FACE ( 'NONE', ( #2658 ), #7554, .T. ) ;
#9899 = CARTESIAN_POINT ( 'NONE',  ( -8.080465354403331801, 46.01554175503538602, 75.45433879953087342 ) ) ;
#9900 = CARTESIAN_POINT ( 'NONE',  ( 5.008975552073978932, 51.78836144432716537, 77.68963291717794561 ) ) ;
#9901 = EDGE_CURVE ( 'NONE', #7818, #11295, #5951, .T. ) ;
#9902 = CARTESIAN_POINT ( 'NONE',  ( 2.029186242314200861, 35.35002428291939225, 76.16022115247204738 ) ) ;
#9903 = CARTESIAN_POINT ( 'NONE',  ( -5.160557796315992540, 37.41935686500602287, 77.33669174070733732 ) ) ;
#9904 = CARTESIAN_POINT ( 'NONE',  ( -5.616286711741430793, 44.43019146960381960, 93.73558879782399345 ) ) ;
#9905 = DIRECTION ( 'NONE',  ( -1.110223024625156540E-16, -1.000000000000000000, -5.922860397471808077E-17 ) ) ;
#9906 = CARTESIAN_POINT ( 'NONE',  ( 9.341681937738675501, 42.79133789484158967, 77.50995918449682165 ) ) ;
#9907 = CARTESIAN_POINT ( 'NONE',  ( -3.059371429944726550, 36.79212808410388647, 76.40804902690982203 ) ) ;
#9908 = CARTESIAN_POINT ( 'NONE',  ( -4.406172944158208260, 37.61675910519541333, 75.97348137399042400 ) ) ;
#9909 = CARTESIAN_POINT ( 'NONE',  ( 6.198496396448986090, 45.68315280215533392, 91.58621380123798872 ) ) ;
#9910 = ORIENTED_EDGE ( 'NONE', *, *, #4239, .F. ) ;
#9911 = CARTESIAN_POINT ( 'NONE',  ( 8.792941515635110505, 41.14672803835393466, 78.80099766627323277 ) ) ;
#9912 = CARTESIAN_POINT ( 'NONE',  ( -7.154059339130676598, 47.04588606493869918, 77.58227997600145898 ) ) ;
#9913 = CARTESIAN_POINT ( 'NONE',  ( -4.879976564110340753, 37.21210281127717678, 78.77850703318271997 ) ) ;
#9914 = LINE ( 'NONE', #3295, #2736 ) ;
#9915 = EDGE_CURVE ( 'NONE', #8877, #895, #4345, .T. ) ;
#9916 = CARTESIAN_POINT ( 'NONE',  ( 8.677276008184190204, 40.80007117484056067, 75.42295143068700725 ) ) ;
#9917 = ORIENTED_EDGE ( 'NONE', *, *, #5062, .T. ) ;
#9918 = CARTESIAN_POINT ( 'NONE',  ( 6.339841751912436152, 38.42329159016732376, 75.87985893138584004 ) ) ;
#9919 = VECTOR ( 'NONE', #5757, 1000.000000000000000 ) ;
#9920 = CARTESIAN_POINT ( 'NONE',  ( 0.07956630390167138134, 52.97185586811492897, 79.50648293536016809 ) ) ;
#9921 = CARTESIAN_POINT ( 'NONE',  ( 6.663926478743484871, 37.73509508818325031, 78.14418354478426920 ) ) ;
#9922 = CARTESIAN_POINT ( 'NONE',  ( -3.674734132037354772, 36.32183877683145568, 75.77010869825431882 ) ) ;
#9923 = EDGE_CURVE ( 'NONE', #5122, #3672, #8579, .T. ) ;
#9924 = FACE_OUTER_BOUND ( 'NONE', #9733, .T. ) ;
#9925 = ORIENTED_EDGE ( 'NONE', *, *, #13030, .T. ) ;
#9926 = AXIS2_PLACEMENT_3D ( 'NONE', #19824, #18031, #9964 ) ;
#9927 = CARTESIAN_POINT ( 'NONE',  ( -4.491212578019011303, 51.39558556899189057, 78.91875292420674270 ) ) ;
#9928 = EDGE_CURVE ( 'NONE', #5725, #10089, #1488, .T. ) ;
#9929 = ORIENTED_EDGE ( 'NONE', *, *, #6614, .T. ) ;
#9930 = CARTESIAN_POINT ( 'NONE',  ( 6.198496396448986090, 45.68315280215533392, 91.58621380123798872 ) ) ;
#9931 = CARTESIAN_POINT ( 'NONE',  ( 1.633003964141607867, 52.20540239326999910, 76.88486154722851040 ) ) ;
#9932 = PLANE ( 'NONE',  #20515 ) ;
#9933 = AXIS2_PLACEMENT_3D ( 'NONE', #953, #4136, #10449 ) ;
#9934 = CARTESIAN_POINT ( 'NONE',  ( 13.32277635493563039, 36.96218137147968008, 54.55433879953099563 ) ) ;
#9935 = ORIENTED_EDGE ( 'NONE', *, *, #14019, .F. ) ;
#9936 = VECTOR ( 'NONE', #8031, 1000.000000000000000 ) ;
#9937 = DIRECTION ( 'NONE',  ( 0.000000000000000000, 1.734723475976787846E-14, -1.000000000000000000 ) ) ;
#9938 = ORIENTED_EDGE ( 'NONE', *, *, #12225, .F. ) ;
#9939 = LINE ( 'NONE', #16423, #2380 ) ;
#9940 = LINE ( 'NONE', #14808, #20094 ) ;
#9941 = CARTESIAN_POINT ( 'NONE',  ( 4.470572738639666532, 36.16780480931087283, 79.45433879953087342 ) ) ;
#9942 = ORIENTED_EDGE ( 'NONE', *, *, #4257, .F. ) ;
#9943 = CARTESIAN_POINT ( 'NONE',  ( 5.434012744193106315, 45.09686908721048582, 92.45433879953098710 ) ) ;
#9944 = CARTESIAN_POINT ( 'NONE',  ( 8.559588968570775336, 45.78687671259945802, 75.44992703482499508 ) ) ;
#9945 = CARTESIAN_POINT ( 'NONE',  ( -5.838428831739583380, 50.43291415881836315, 78.10580938776615767 ) ) ;
#9946 = DIRECTION ( 'NONE',  ( -0.3165065846431827090, -0.9485903129789527988, 0.000000000000000000 ) ) ;
#9947 = ADVANCED_FACE ( 'NONE', ( #11388 ), #3283, .T. ) ;
#9948 = CARTESIAN_POINT ( 'NONE',  ( 8.889576793745449734, 46.88836537034026719, 78.73595644658969661 ) ) ;
#9949 = ORIENTED_EDGE ( 'NONE', *, *, #15786, .T. ) ;
#9950 = CARTESIAN_POINT ( 'NONE',  ( -4.039182523966593052, 50.97167426352094566, 76.19049300047602458 ) ) ;
#9951 = CARTESIAN_POINT ( 'NONE',  ( 23.63948732994508006, 36.35905713404685002, 76.90433879953101837 ) ) ;
#9952 = AXIS2_PLACEMENT_3D ( 'NONE', #21032, #6468, #12973 ) ;
#9953 = ORIENTED_EDGE ( 'NONE', *, *, #3004, .T. ) ;
#9954 = CARTESIAN_POINT ( 'NONE',  ( 4.890314246961300348, 51.87601177044496836, 77.76130678786321937 ) ) ;
#9955 = CARTESIAN_POINT ( 'NONE',  ( 2.122153740306507608, 50.16218137147969713, 85.55433879953100984 ) ) ;
#9956 = VECTOR ( 'NONE', #12554, 1000.000000000000000 ) ;
#9957 = CYLINDRICAL_SURFACE ( 'NONE', #20373, 5.199999999999999289 ) ;
#9958 = CARTESIAN_POINT ( 'NONE',  ( 4.512269934384613101, 47.81844922806527620, 95.06371379611701400 ) ) ;
#9959 = CARTESIAN_POINT ( 'NONE',  ( -1.876873622437039701, 39.01745058958429269, 93.96996379782397923 ) ) ;
#9960 = CARTESIAN_POINT ( 'NONE',  ( 5.490969714706527505, 37.64385856151075416, 76.26708001093082601 ) ) ;
#9961 = CARTESIAN_POINT ( 'NONE',  ( -1.477846259693490705, 49.81903562097208038, 61.15433879953099705 ) ) ;
#9962 = VERTEX_POINT ( 'NONE', #14770 ) ;
#9963 = DIRECTION ( 'NONE',  ( -1.779391786395883536E-16, -5.922860397471806844E-17, 1.000000000000000000 ) ) ;
#9964 = DIRECTION ( 'NONE',  ( 1.000000000000000000, 0.000000000000000000, 0.000000000000000000 ) ) ;
#9965 = ORIENTED_EDGE ( 'NONE', *, *, #15096, .F. ) ;
#9966 = VECTOR ( 'NONE', #18403, 1000.000000000000000 ) ;
#9967 = CARTESIAN_POINT ( 'NONE',  ( -1.219056181836354558, 49.77488197367695477, 93.31237966814926210 ) ) ;
#9968 = EDGE_CURVE ( 'NONE', #20977, #5606, #4249, .T. ) ;
#9969 = CARTESIAN_POINT ( 'NONE',  ( -0.02883801100815608018, 35.36625256049322275, 79.45433879953087342 ) ) ;
#9970 = CARTESIAN_POINT ( 'NONE',  ( -0.2125050281363792815, 38.58189400963055959, 94.24246379953099506 ) ) ;
#9971 = ORIENTED_EDGE ( 'NONE', *, *, #3859, .F. ) ;
#9972 = LINE ( 'NONE', #13557, #8863 ) ;
#9973 = CARTESIAN_POINT ( 'NONE',  ( -5.772695632942807187, 37.87151842650609268, 75.75097338717934292 ) ) ;
#9974 = ORIENTED_EDGE ( 'NONE', *, *, #19722, .F. ) ;
#9975 = CARTESIAN_POINT ( 'NONE',  ( 5.599886173630381769, 51.35187957151522653, 78.68193220087633222 ) ) ;
#9976 = CARTESIAN_POINT ( 'NONE',  ( 0.3332310122597790802, 52.96015324592079310, 76.34474143055572881 ) ) ;
#9977 = CARTESIAN_POINT ( 'NONE',  ( -3.981178359372548492, 46.76218137147973408, 92.60183879953099506 ) ) ;
#9978 = ORIENTED_EDGE ( 'NONE', *, *, #1305, .T. ) ;
#9979 = CARTESIAN_POINT ( 'NONE',  ( -4.578768572918487045, 36.98961260158169040, 78.00876120161012750 ) ) ;
#9980 = PRODUCT_DEFINITION_CONTEXT ( 'detailed design', #9148, 'design' ) ;
#9981 = ORIENTED_EDGE ( 'NONE', *, *, #20288, .T. ) ;
#9982 = CARTESIAN_POINT ( 'NONE',  ( 8.449576249518734983, 46.30180237598475657, 78.74038740353792321 ) ) ;
#9983 = LINE ( 'NONE', #14544, #2972 ) ;
#9984 = DIRECTION ( 'NONE',  ( 0.000000000000000000, 0.000000000000000000, -1.000000000000000000 ) ) ;
#9985 = CARTESIAN_POINT ( 'NONE',  ( -4.524181921268124462, 40.28999182795290324, 94.78933880123798872 ) ) ;
#9986 = VECTOR ( 'NONE', #11903, 1000.000000000000114 ) ;
#9987 = CARTESIAN_POINT ( 'NONE',  ( -42.80431130087157499, 52.72888056379152744, -8.100000000000003197 ) ) ;
#9988 = EDGE_CURVE ( 'NONE', #10468, #13576, #19248, .T. ) ;
#9989 = DIRECTION ( 'NONE',  ( -1.540237394707284220E-16, -1.793354297423764243E-16, 1.000000000000000000 ) ) ;
#9990 = CARTESIAN_POINT ( 'NONE',  ( 4.055885703770254480, 36.79126021913294409, 75.97723610431854979 ) ) ;
#9991 = FACE_OUTER_BOUND ( 'NONE', #12290, .T. ) ;
#9992 = ORIENTED_EDGE ( 'NONE', *, *, #7560, .T. ) ;
#9993 = LINE ( 'NONE', #10090, #14927 ) ;
#9994 = CARTESIAN_POINT ( 'NONE',  ( 8.643719690846561221, 43.06391881351956386, 76.64232882509132594 ) ) ;
#9995 = CYLINDRICAL_SURFACE ( 'NONE', #2818, 0.5999999999999894307 ) ;
#9996 = CARTESIAN_POINT ( 'NONE',  ( 6.634437729966897734, 50.58769801112816111, 77.73730439759678745 ) ) ;
#9997 =( BOUNDED_SURFACE ( )  B_SPLINE_SURFACE ( 1, 2, ( 
 ( #13802, #12528, #14018, #19015, #20279, #18700, #6138, #15516, #17318, #2742, #930, #12329, #2945, #15412, #10950, #9246, #15733, #1151, #827, #17422, #5709, #12216, #12641, #11052, #17524, #14541, #14434, #20905, #19429, #4847, #1466, #3165, #19532, #6656, #8265, #21005, #16354, #9871, #19633, #9451, #18048, #6440, #6335, #11367, #1357, #12838, #4948, #1785, #1671, #19217, #11573, #19317, #13158, #16045, #5054, #4632, #17836, #20810, #13058, #7849, #9763 ),
 ( #7951, #4733, #14334, #3053, #11263, #6237, #11153, #17621, #9562, #3264, #17940, #3361, #1568, #8053, #17734, #9667, #16148, #12949, #9301, #12583, #4483, #5773, #4270, #7688, #1100, #17475, #2582, #12280, #8980, #18760, #9083, #986, #20452, #7476, #13970, #7589, #4374, #13699, #1144, #9343, #62, #6646, #10612, #7282, #5905, #7606, #18664, #19091, #20357, #1217, #17180, #5999, #15486, #7385, #1005, #2506, #8999, #7706, #2916, #13988, #9100 ) ),
 .UNSPECIFIED., .F., .F., .F. ) 
 B_SPLINE_SURFACE_WITH_KNOTS ( ( 2, 2 ),
 ( 3, 2, 2, 2, 2, 2, 2, 2, 2, 2, 2, 2, 2, 2, 2, 2, 2, 2, 2, 2, 2, 2, 2, 2, 2, 2, 2, 2, 2, 2, 3 ),
 ( 0.000000000000000000, 1.000000000000000000 ),
 ( 0.000000000000000000, 0.03125000000000000000, 0.06250000000000000000, 0.09375000000000000000, 0.1250000000000000000, 0.1562500000000000000, 0.1875000000000000000, 0.2187500000000000000, 0.2500000000000000000, 0.2812500000000000000, 0.3125000000000000000, 0.3437500000000000000, 0.3750000000000000000, 0.4062500000000000000, 0.4375000000000000000, 0.4687500000000000000, 0.5000000000000000000, 0.5312500000000000000, 0.5625000000000000000, 0.5937500000000000000, 0.6250000000000000000, 0.6562500000000000000, 0.6875000000000000000, 0.7187500000000000000, 0.7500000000000000000, 0.7812500000000000000, 0.8125000000000000000, 0.8437500000000000000, 0.8750000000000000000, 0.9062500000000000000, 0.9200238733485665010 ),
 .UNSPECIFIED. ) 
 GEOMETRIC_REPRESENTATION_ITEM ( )  RATIONAL_B_SPLINE_SURFACE ( (
 ( 1.000000000000000000, 0.9238795325112867385, 1.000000000000000000, 0.9238795325112867385, 1.000000000000000000, 0.9238795325112867385, 1.000000000000000000, 0.9238795325112867385, 1.000000000000000000, 0.9238795325112867385, 1.000000000000000000, 0.9238795325112867385, 1.000000000000000000, 0.9238795325112867385, 1.000000000000000000, 0.9238795325112867385, 1.000000000000000000, 0.9238795325112867385, 1.000000000000000000, 0.9238795325112867385, 1.000000000000000000, 0.9238795325112867385, 1.000000000000000000, 0.9238795325112867385, 1.000000000000000000, 0.9238795325112867385, 1.000000000000000000, 0.9238795325112867385, 1.000000000000000000, 0.9238795325112867385, 1.000000000000000000, 0.9238795325112867385, 1.000000000000000000, 0.9238795325112867385, 1.000000000000000000, 0.9238795325112867385, 1.000000000000000000, 0.9238795325112867385, 1.000000000000000000, 0.9238795325112867385, 1.000000000000000000, 0.9238795325112867385, 1.000000000000000000, 0.9238795325112867385, 1.000000000000000000, 0.9238795325112867385, 1.000000000000000000, 0.9238795325112867385, 1.000000000000000000, 0.9238795325112867385, 1.000000000000000000, 0.9238795325112867385, 1.000000000000000000, 0.9238795325112867385, 1.000000000000000000, 0.9238795325112867385, 1.000000000000000000, 0.9238795325112867385, 1.000000000000000000, 0.9664488422904572440, 0.9624739659882119991),
 ( 1.000000000000000000, 0.9238795325112867385, 1.000000000000000000, 0.9238795325112867385, 1.000000000000000000, 0.9238795325112867385, 1.000000000000000000, 0.9238795325112867385, 1.000000000000000000, 0.9238795325112867385, 1.000000000000000000, 0.9238795325112867385, 1.000000000000000000, 0.9238795325112867385, 1.000000000000000000, 0.9238795325112867385, 1.000000000000000000, 0.9238795325112867385, 1.000000000000000000, 0.9238795325112867385, 1.000000000000000000, 0.9238795325112867385, 1.000000000000000000, 0.9238795325112867385, 1.000000000000000000, 0.9238795325112867385, 1.000000000000000000, 0.9238795325112867385, 1.000000000000000000, 0.9238795325112867385, 1.000000000000000000, 0.9238795325112867385, 1.000000000000000000, 0.9238795325112867385, 1.000000000000000000, 0.9238795325112867385, 1.000000000000000000, 0.9238795325112867385, 1.000000000000000000, 0.9238795325112867385, 1.000000000000000000, 0.9238795325112867385, 1.000000000000000000, 0.9238795325112867385, 1.000000000000000000, 0.9238795325112867385, 1.000000000000000000, 0.9238795325112867385, 1.000000000000000000, 0.9238795325112867385, 1.000000000000000000, 0.9238795325112867385, 1.000000000000000000, 0.9238795325112867385, 1.000000000000000000, 0.9238795325112867385, 1.000000000000000000, 0.9238795325112867385, 1.000000000000000000, 0.9664488422904572440, 0.9624739659882119991) ) ) 
 REPRESENTATION_ITEM ( '' )  SURFACE ( )  );
#9998 = ORIENTED_EDGE ( 'NONE', *, *, #3974, .T. ) ;
#9999 = CIRCLE ( 'NONE', #1833, 3.999999999999996447 ) ;
#10000 = EDGE_CURVE ( 'NONE', #20886, #12245, #10361, .T. ) ;
#10001 = DIRECTION ( 'NONE',  ( -0.8043570849667761591, 0.5941461771851690443, -1.733862608106491891E-17 ) ) ;
#10002 = ORIENTED_EDGE ( 'NONE', *, *, #19772, .T. ) ;
#10003 = CARTESIAN_POINT ( 'NONE',  ( 5.722153675945192752, 44.84677459913377362, 93.67075777718372365 ) ) ;
#10004 = LINE ( 'NONE', #12970, #20626 ) ;
#10005 = CARTESIAN_POINT ( 'NONE',  ( -0.2286725555534918908, 52.93086078304144593, 75.48599683584926368 ) ) ;
#10006 = PLANE ( 'NONE',  #90 ) ;
#10007 = CARTESIAN_POINT ( 'NONE',  ( 5.856396280011939126, 46.10368687828906076, 94.43871379782397923 ) ) ;
#10008 = CARTESIAN_POINT ( 'NONE',  ( 4.394343283833276104, 39.11584570990505938, 93.85183880123807398 ) ) ;
#10009 = CARTESIAN_POINT ( 'NONE',  ( 4.591779561242093521, 52.09652731707507201, 76.01224951307210631 ) ) ;
#10010 = CARTESIAN_POINT ( 'NONE',  ( 6.882736312352589536, 37.89144858414100270, 76.69330938776616335 ) ) ;
#10011 = CARTESIAN_POINT ( 'NONE',  ( -5.784195910403845176, 44.99242805365518194, 90.88308880123798872 ) ) ;
#10012 = CARTESIAN_POINT ( 'NONE',  ( -2.416137431568557314, 39.07291177436112406, 93.61746380123797451 ) ) ;
#10013 = ORIENTED_EDGE ( 'NONE', *, *, #2246, .F. ) ;
#10014 = CARTESIAN_POINT ( 'NONE',  ( 0.3346339570403927821, 52.96754328674535373, 76.26461983994238381 ) ) ;
#10015 = DIRECTION ( 'NONE',  ( 1.540237394707284220E-16, 1.793354297423764243E-16, -1.000000000000000000 ) ) ;
#10016 = CARTESIAN_POINT ( 'NONE',  ( 2.522153740306509739, 50.16218137147969713, 59.55433879953099563 ) ) ;
#10017 = CARTESIAN_POINT ( 'NONE',  ( 25.63948732994507651, 43.16218137147969003, 74.70433879953100131 ) ) ;
#10018 = CARTESIAN_POINT ( 'NONE',  ( 9.292527943876132568, 42.64402025696431764, 77.82525376769920911 ) ) ;
#10019 = ORIENTED_EDGE ( 'NONE', *, *, #2496, .T. ) ;
#10020 = VERTEX_POINT ( 'NONE', #4757 ) ;
#10021 = DIRECTION ( 'NONE',  ( -4.731737692062757470E-17, 0.7071067811865512365, 0.7071067811865439090 ) ) ;
#10022 = CARTESIAN_POINT ( 'NONE',  ( 7.680032241523795378, 40.16158449578585277, 77.69330938776616335 ) ) ;
#10023 = CARTESIAN_POINT ( 'NONE',  ( -3.763323997310421554, 36.38727654169122161, 75.66260743385902288 ) ) ;
#10024 = PLANE ( 'NONE',  #8583 ) ;
#10025 = VERTEX_POINT ( 'NONE', #19760 ) ;
#10026 = DIRECTION ( 'NONE',  ( -0.5941461771851693774, -0.8043570849667760481, -2.357623395011396791E-16 ) ) ;
#10027 = CARTESIAN_POINT ( 'NONE',  ( 9.273778039597953438, 45.67340037358405169, 78.74919174070734584 ) ) ;
#10028 = VERTEX_POINT ( 'NONE', #9899 ) ;
#10029 = CARTESIAN_POINT ( 'NONE',  ( -5.784195910403845176, 44.99242805365518194, 90.88308880123798872 ) ) ;
#10030 = EDGE_CURVE ( 'NONE', #16818, #20921, #16627, .T. ) ;
#10031 = CARTESIAN_POINT ( 'NONE',  ( 1.822474108708594720, 52.20390835154866238, 76.99833242929096855 ) ) ;
#10032 = ADVANCED_FACE ( 'NONE', ( #1902 ), #8391, .F. ) ;
#10033 = CARTESIAN_POINT ( 'NONE',  ( -2.416137431568557314, 39.07291177436112406, 96.11746380123797451 ) ) ;
#10034 = CARTESIAN_POINT ( 'NONE',  ( 6.882736312352589536, 37.89144858414100270, 77.26022115247205591 ) ) ;
#10035 = VERTEX_POINT ( 'NONE', #6675 ) ;
#10036 = EDGE_CURVE ( 'NONE', #11820, #5798, #16415, .T. ) ;
#10037 = CARTESIAN_POINT ( 'NONE',  ( 1.771153339986189845, 40.36218137147969998, 46.35433879953098568 ) ) ;
#10038 = ADVANCED_FACE ( 'NONE', ( #20071 ), #11907, .T. ) ;
#10039 = ORIENTED_EDGE ( 'NONE', *, *, #6763, .T. ) ;
#10040 = CARTESIAN_POINT ( 'NONE',  ( -1.535769738210056357, 49.45816841730323432, 93.04858131124048271 ) ) ;
#10041 = CARTESIAN_POINT ( 'NONE',  ( -4.901157372041539340, 42.48549306292126460, 95.05433879953096721 ) ) ;
#10042 = EDGE_CURVE ( 'NONE', #14796, #20391, #2114, .T. ) ;
#10043 = VERTEX_POINT ( 'NONE', #7089 ) ;
#10044 = CARTESIAN_POINT ( 'NONE',  ( 5.220616844236031007, 45.87228208810806507, 92.48558879611698558 ) ) ;
#10045 = CARTESIAN_POINT ( 'NONE',  ( 8.095626740731175275, 41.43801618066453329, 75.36738766396204880 ) ) ;
#10046 = CARTESIAN_POINT ( 'NONE',  ( -4.477846259693478714, 37.66295064777091994, 53.55433879953098852 ) ) ;
#10047 = CARTESIAN_POINT ( 'NONE',  ( -4.383821200644077543, 51.47232351541473605, 78.52322435057745054 ) ) ;
#10048 = CARTESIAN_POINT ( 'NONE',  ( -4.009385194876761815, 46.27527268018315709, 93.26683879953097289 ) ) ;
#10049 = EDGE_LOOP ( 'NONE', ( #3319, #14968, #12915, #6224, #8433 ) ) ;
#10050 = B_SPLINE_CURVE_WITH_KNOTS ( 'NONE', 3,
 ( #8227, #14714, #19593, #11533, #5015, #660, #18319, #13435, #20003, #16629, #2050, #15244 ),
 .UNSPECIFIED., .F., .F.,
 ( 4, 2, 2, 2, 2, 4 ),
 ( 0.000000000000000000, 0.0001072365356795881180, 0.0002144730713591762360, 0.0004289461427183928585, 0.0006434192140776094811, 0.0008578922854368260494 ),
 .UNSPECIFIED. ) ;
#10051 = CARTESIAN_POINT ( 'NONE',  ( -2.393324858630934138, 39.09930439799452984, 92.55433879953105247 ) ) ;
#10052 = VERTEX_POINT ( 'NONE', #8710 ) ;
#10053 = DIRECTION ( 'NONE',  ( -1.402518428993830937E-16, 1.000000000000000000, -3.469446951953617147E-16 ) ) ;
#10054 = CARTESIAN_POINT ( 'NONE',  ( -6.714292542261278030, 40.32675560908123913, 78.24455606223649795 ) ) ;
#10055 = DIRECTION ( 'NONE',  ( -1.779391786395883536E-16, -5.922860397471806844E-17, 1.000000000000000000 ) ) ;
#10056 = CARTESIAN_POINT ( 'NONE',  ( 2.635245049009968810, 48.69372030666295359, 93.89183879611699979 ) ) ;
#10057 = DIRECTION ( 'NONE',  ( -1.540237394707283727E-16, -1.793354297423763257E-16, 1.000000000000000000 ) ) ;
#10058 = CARTESIAN_POINT ( 'NONE',  ( -1.876873622437038369, 39.01745058958429269, 91.46996379782397923 ) ) ;
#10059 = CARTESIAN_POINT ( 'NONE',  ( 5.840776426723270021, 37.14690219845653019, 76.14207271482608519 ) ) ;
#10060 = CARTESIAN_POINT ( 'NONE',  ( -7.496206882273947159, 47.93002185485102018, 78.32480289656686523 ) ) ;
#10061 = VERTEX_POINT ( 'NONE', #11798 ) ;
#10062 = EDGE_CURVE ( 'NONE', #2511, #11695, #15172, .T. ) ;
#10063 = CARTESIAN_POINT ( 'NONE',  ( 0.5221537403065019678, 44.16218137147968292, 72.45433879953087342 ) ) ;
#10064 = CARTESIAN_POINT ( 'NONE',  ( 5.031028746841824884, 37.32608482280444662, 78.09625056423674039 ) ) ;
#10065 = ORIENTED_EDGE ( 'NONE', *, *, #18098, .T. ) ;
#10066 = FACE_OUTER_BOUND ( 'NONE', #6623, .T. ) ;
#10067 = CARTESIAN_POINT ( 'NONE',  ( 2.568262918966977004, 49.46998271715920481, 92.90703276401609401 ) ) ;
#10068 = CARTESIAN_POINT ( 'NONE',  ( -0.2125050281363792815, 38.58189400963055959, 92.99246379953098085 ) ) ;
#10069 = B_SPLINE_SURFACE_WITH_KNOTS ( 'NONE', 3, 1, ( 
 ( #2449, #7332 ),
 ( #5731, #7549 ),
 ( #13933, #12446 ),
 ( #15535, #15647 ),
 ( #14238, #1266 ),
 ( #9368, #2868 ),
 ( #15851, #952 ),
 ( #6049, #15431 ),
 ( #7656, #4342 ),
 ( #20302, #20719 ),
 ( #2552, #5846 ),
 ( #9047, #10867 ),
 ( #20618, #7441 ),
 ( #20416, #18830 ),
 ( #1064, #20521 ),
 ( #12549, #17444 ),
 ( #6432, #4237 ),
 ( #10764, #5948 ),
 ( #12941, #2766 ) ),
 .UNSPECIFIED., .F., .F., .F.,
 ( 4, 1, 1, 1, 1, 1, 1, 1, 1, 1, 1, 1, 1, 1, 1, 1, 4 ),
 ( 2, 2 ),
 ( 0.000000000000000000, 0.07118833779177360932, 0.1347494984424237596, 0.1905117199385542026, 0.2387103502848646475, 0.2842577524993954441, 0.3323041331166366463, 0.3837985941886438157, 0.4397333780097005262, 0.4984292962743230304, 0.5584994700834656767, 0.6208277070730616742, 0.6868513727233629407, 0.7572275588454563389, 0.8323608126527687334, 0.9133389214536370426, 1.000000000000000000 ),
 ( 0.000000000000000000, 1.000000000000000000 ),
 .UNSPECIFIED. ) ;
#10070 = ORIENTED_EDGE ( 'NONE', *, *, #6772, .F. ) ;
#10071 = CARTESIAN_POINT ( 'NONE',  ( 8.787829143201870252, 41.13140593384865440, 77.80727997600146750 ) ) ;
#10072 = CARTESIAN_POINT ( 'NONE',  ( -5.955289093497887265, 38.00639286050488153, 76.68644156968609593 ) ) ;
#10073 = VERTEX_POINT ( 'NONE', #18493 ) ;
#10074 = FACE_OUTER_BOUND ( 'NONE', #7905, .T. ) ;
#10075 = CARTESIAN_POINT ( 'NONE',  ( 0.4484089342563315483, 52.96189929305592869, 75.99664213318317252 ) ) ;
#10076 = ORIENTED_EDGE ( 'NONE', *, *, #5316, .F. ) ;
#10077 = CARTESIAN_POINT ( 'NONE',  ( -4.347163611243005654, 37.59329646478425246, 77.92182307551118470 ) ) ;
#10078 = EDGE_LOOP ( 'NONE', ( #11145, #7039, #13549, #2078 ) ) ;
#10079 = CARTESIAN_POINT ( 'NONE',  ( -4.699529792962120034, 51.24672971417357559, 75.98997946140892168 ) ) ;
#10080 = FACE_OUTER_BOUND ( 'NONE', #15979, .T. ) ;
#10081 = CARTESIAN_POINT ( 'NONE',  ( -0.9988176903691428077, 49.83852402762217082, 94.39871380123798872 ) ) ;
#10082 = DIRECTION ( 'NONE',  ( 0.000000000000000000, 0.000000000000000000, 1.000000000000000000 ) ) ;
#10083 = CARTESIAN_POINT ( 'NONE',  ( 6.253655717016493476, 49.94413339827291765, 75.66183449524544358 ) ) ;
#10084 = CARTESIAN_POINT ( 'NONE',  ( -5.955451856753747997, 38.00651308716548726, 78.53742703482498655 ) ) ;
#10085 = DIRECTION ( 'NONE',  ( -1.540237394707284220E-16, -1.793354297423764243E-16, 1.000000000000000000 ) ) ;
#10086 = EDGE_LOOP ( 'NONE', ( #11356, #399, #12052, #17516, #12548 ) ) ;
#10087 = CARTESIAN_POINT ( 'NONE',  ( 3.975681152273106367, 36.73394898310913703, 76.35980278528342069 ) ) ;
#10088 = CARTESIAN_POINT ( 'NONE',  ( 8.394097411062748648, 39.95136695475236621, 78.67376765716130649 ) ) ;
#10089 = VERTEX_POINT ( 'NONE', #18176 ) ;
#10090 = CARTESIAN_POINT ( 'NONE',  ( 31.03948732994507864, 36.35905713404685002, 78.30433879953099563 ) ) ;
#10091 = CARTESIAN_POINT ( 'NONE',  ( 9.009194133669925719, 41.79485085341455886, 75.38196330830126612 ) ) ;
#10092 = CARTESIAN_POINT ( 'NONE',  ( 0.3869120917952211802, 35.96329670974014192, 76.86610350541323555 ) ) ;
#10093 = FACE_OUTER_BOUND ( 'NONE', #12871, .T. ) ;
#10094 = ORIENTED_EDGE ( 'NONE', *, *, #2222, .T. ) ;
#10095 = EDGE_LOOP ( 'NONE', ( #20040, #4785, #822, #4088 ) ) ;
#10096 = AXIS2_PLACEMENT_3D ( 'NONE', #21009, #11370, #13061 ) ;
#10097 = FACE_OUTER_BOUND ( 'NONE', #10095, .T. ) ;
#10098 = ORIENTED_EDGE ( 'NONE', *, *, #7551, .F. ) ;
#10099 = CARTESIAN_POINT ( 'NONE',  ( -3.711266317373841161, 36.34882363053332455, 77.55767546204062057 ) ) ;
#10100 = EDGE_CURVE ( 'NONE', #16102, #4527, #3592, .T. ) ;
#10101 = DIRECTION ( 'NONE',  ( -1.110223024625156540E-16, -1.000000000000000000, -5.922860397471808077E-17 ) ) ;
#10102 = CARTESIAN_POINT ( 'NONE',  ( 4.668718747243733702, 52.03969543967511413, 77.44183710417100031 ) ) ;
#10103 = CARTESIAN_POINT ( 'NONE',  ( 2.484494565094233831, 50.04344131194918788, 72.45433879953087342 ) ) ;
#10104 = CARTESIAN_POINT ( 'NONE',  ( -4.901157372041539340, 42.48549306292126460, 95.05433879953096721 ) ) ;
#10105 = CARTESIAN_POINT ( 'NONE',  ( 8.211361072458180033, 41.32375023436543415, 76.40801527011910821 ) ) ;
#10106 = CARTESIAN_POINT ( 'NONE',  ( 8.661599634585137153, 45.15687757339797059, 72.45433879953087342 ) ) ;
#10107 = DIRECTION ( 'NONE',  ( -0.5941461771851693774, -0.8043570849667760481, -2.357623395011396791E-16 ) ) ;
#10108 = CARTESIAN_POINT ( 'NONE',  ( -3.943187491250720544, 40.73580453397070755, 95.64871380294496817 ) ) ;
#10109 = VECTOR ( 'NONE', #15255, 1000.000000000000000 ) ;
#10110 = CARTESIAN_POINT ( 'NONE',  ( 3.460444912181559474, 49.25145096859824889, 90.49246380123798872 ) ) ;
#10111 = EDGE_LOOP ( 'NONE', ( #10632, #14849, #12930, #17795 ) ) ;
#10112 = FACE_OUTER_BOUND ( 'NONE', #20155, .T. ) ;
#10113 =( BOUNDED_SURFACE ( )  B_SPLINE_SURFACE ( 1, 2, ( 
 ( #15793, #18965, #19170, #11106, #5890, #18865, #17574, #4378, #20558, #10904, #7691, #9088, #17268, #9199, #20651, #6081, #12588, #19077, #4486, #11007, #17479, #9401, #17788, #6390, #20079, #11206, #1908, #18281, #3502, #2221, #17680, #11709, #3109, #9612, #16094, #15202, #14488, #16591, #2011, #616, #10221, #19870, #301, #16699, #6989, #4792, #20956, #3699, #15104, #8509, #11917, #5191, #1517, #8002, #16488, #6898, #12894, #8400, #512, #3812, #2122, #19376, #19968, #7096, #11314, #14879, #8718, #10011, #413, #6792, #8622, #13299, #11805, #19770, #18184, #13494, #3601, #14994, #13401 ),
 ( #13601, #10108, #5291, #5395, #18391, #10331, #16803, #18709, #17328, #13921, #12439, #8933, #10755, #18917, #5942, #2323, #20289, #2646, #5721, #7539, #5617, #12026, #14127, #9257, #4332, #939, #18500, #1161, #10859, #2541, #12122, #4122, #7211, #5515, #15525, #4229, #20403, #3912, #2754, #7647, #8819, #15744, #10537, #10438, #15316, #16901, #836, #15421, #728, #13712, #20187, #7427, #18603, #4016, #17007, #2437, #7321, #13811, #12226, #10652, #17118, #9038, #5833, #15635, #12339, #18819, #17220, #9145, #1055, #14030, #20511, #8161, #19224, #20912, #4546, #8059, #1365, #12848, #3173 ) ),
 .UNSPECIFIED., .F., .F., .F. ) 
 B_SPLINE_SURFACE_WITH_KNOTS ( ( 2, 2 ),
 ( 3, 2, 2, 2, 2, 2, 2, 2, 2, 2, 2, 2, 2, 2, 2, 2, 2, 2, 2, 2, 2, 2, 2, 2, 2, 2, 2, 2, 2, 2, 2, 2, 2, 2, 2, 2, 2, 2, 2, 3 ),
 ( 0.000000000000000000, 1.000000000000000000 ),
 ( 0.000000000000000000, 0.02500000000000000139, 0.05000000000000000278, 0.07499999999999999722, 0.1000000000000000056, 0.1250000000000000000, 0.1499999999999999944, 0.1749999999999999889, 0.2000000000000000111, 0.2250000000000000056, 0.2500000000000000000, 0.2750000000000000222, 0.2999999999999999889, 0.3250000000000000111, 0.3499999999999999778, 0.3750000000000000000, 0.4000000000000000222, 0.4249999999999999889, 0.4500000000000000111, 0.4749999999999999778, 0.5000000000000000000, 0.5250000000000000222, 0.5500000000000000444, 0.5749999999999999556, 0.5999999999999999778, 0.6250000000000000000, 0.6500000000000000222, 0.6750000000000000444, 0.6999999999999999556, 0.7249999999999999778, 0.7500000000000000000, 0.7750000000000000222, 0.8000000000000000444, 0.8249999999999999556, 0.8499999999999999778, 0.8750000000000000000, 0.9000000000000000222, 0.9250000000000000444, 0.9499999999999999556, 0.9600309957089442348 ),
 .UNSPECIFIED. ) 
 GEOMETRIC_REPRESENTATION_ITEM ( )  RATIONAL_B_SPLINE_SURFACE ( (
 ( 1.000000000000000000, 0.9238795325112867385, 1.000000000000000000, 0.9238795325112867385, 1.000000000000000000, 0.9238795325112867385, 1.000000000000000000, 0.9238795325112867385, 1.000000000000000000, 0.9238795325112867385, 1.000000000000000000, 0.9238795325112867385, 1.000000000000000000, 0.9238795325112867385, 1.000000000000000000, 0.9238795325112867385, 1.000000000000000000, 0.9238795325112867385, 1.000000000000000000, 0.9238795325112867385, 1.000000000000000000, 0.9238795325112867385, 1.000000000000000000, 0.9238795325112867385, 1.000000000000000000, 0.9238795325112867385, 1.000000000000000000, 0.9238795325112867385, 1.000000000000000000, 0.9238795325112867385, 1.000000000000000000, 0.9238795325112867385, 1.000000000000000000, 0.9238795325112867385, 1.000000000000000000, 0.9238795325112867385, 1.000000000000000000, 0.9238795325112867385, 1.000000000000000000, 0.9238795325112867385, 1.000000000000000000, 0.9238795325112867385, 1.000000000000000000, 0.9238795325112867385, 1.000000000000000000, 0.9238795325112867385, 1.000000000000000000, 0.9238795325112867385, 1.000000000000000000, 0.9238795325112867385, 1.000000000000000000, 0.9238795325112867385, 1.000000000000000000, 0.9238795325112867385, 1.000000000000000000, 0.9238795325112867385, 1.000000000000000000, 0.9238795325112867385, 1.000000000000000000, 0.9238795325112867385, 1.000000000000000000, 0.9238795325112867385, 1.000000000000000000, 0.9238795325112867385, 1.000000000000000000, 0.9238795325112867385, 1.000000000000000000, 0.9238795325112867385, 1.000000000000000000, 0.9238795325112867385, 1.000000000000000000, 0.9238795325112867385, 1.000000000000000000, 0.9238795325112867385, 1.000000000000000000, 0.9238795325112867385, 1.000000000000000000, 0.9694574366903154772, 0.9634246591005992677),
 ( 1.000000000000000000, 0.9238795325112867385, 1.000000000000000000, 0.9238795325112867385, 1.000000000000000000, 0.9238795325112867385, 1.000000000000000000, 0.9238795325112867385, 1.000000000000000000, 0.9238795325112867385, 1.000000000000000000, 0.9238795325112867385, 1.000000000000000000, 0.9238795325112867385, 1.000000000000000000, 0.9238795325112867385, 1.000000000000000000, 0.9238795325112867385, 1.000000000000000000, 0.9238795325112867385, 1.000000000000000000, 0.9238795325112867385, 1.000000000000000000, 0.9238795325112867385, 1.000000000000000000, 0.9238795325112867385, 1.000000000000000000, 0.9238795325112867385, 1.000000000000000000, 0.9238795325112867385, 1.000000000000000000, 0.9238795325112867385, 1.000000000000000000, 0.9238795325112867385, 1.000000000000000000, 0.9238795325112867385, 1.000000000000000000, 0.9238795325112867385, 1.000000000000000000, 0.9238795325112867385, 1.000000000000000000, 0.9238795325112867385, 1.000000000000000000, 0.9238795325112867385, 1.000000000000000000, 0.9238795325112867385, 1.000000000000000000, 0.9238795325112867385, 1.000000000000000000, 0.9238795325112867385, 1.000000000000000000, 0.9238795325112867385, 1.000000000000000000, 0.9238795325112867385, 1.000000000000000000, 0.9238795325112867385, 1.000000000000000000, 0.9238795325112867385, 1.000000000000000000, 0.9238795325112867385, 1.000000000000000000, 0.9238795325112867385, 1.000000000000000000, 0.9238795325112867385, 1.000000000000000000, 0.9238795325112867385, 1.000000000000000000, 0.9238795325112867385, 1.000000000000000000, 0.9238795325112867385, 1.000000000000000000, 0.9238795325112867385, 1.000000000000000000, 0.9238795325112867385, 1.000000000000000000, 0.9238795325112867385, 1.000000000000000000, 0.9694574366903154772, 0.9634246591005992677) ) ) 
 REPRESENTATION_ITEM ( '' )  SURFACE ( )  );
#10114 = DIRECTION ( 'NONE',  ( -1.402518428993830937E-16, 1.000000000000000000, -3.469446951953617147E-16 ) ) ;
#10115 = PLANE ( 'NONE',  #14660 ) ;
#10116 = CARTESIAN_POINT ( 'NONE',  ( 5.396517835962451493, 50.75616155517602834, 78.93669174070734584 ) ) ;
#10117 = CARTESIAN_POINT ( 'NONE',  ( -4.567115856812060670, 47.10047254335474065, 93.46121380123797451 ) ) ;
#10118 = VECTOR ( 'NONE', #3522, 1000.000000000000000 ) ;
#10119 = DIRECTION ( 'NONE',  ( 0.02533578529877050789, 0.9996789974703352843, 1.831801750099146688E-16 ) ) ;
#10120 = PLANE ( 'NONE',  #19448 ) ;
#10121 = CARTESIAN_POINT ( 'NONE',  ( -1.883296302981685599, 36.95289499283964574, 72.45433879953085921 ) ) ;
#10122 = ORIENTED_EDGE ( 'NONE', *, *, #10682, .F. ) ;
#10123 = ORIENTED_EDGE ( 'NONE', *, *, #4160, .F. ) ;
#10124 = MECHANICAL_DESIGN_GEOMETRIC_PRESENTATION_REPRESENTATION (  '', ( #11146 ), #19275 ) ;
#10125 = ADVANCED_FACE ( 'NONE', ( #721 ), #403, .F. ) ;
#10126 = CARTESIAN_POINT ( 'NONE',  ( 7.721391190447019603, 40.23635033321865961, 78.89153941383322888 ) ) ;
#10127 = CARTESIAN_POINT ( 'NONE',  ( 4.535172733565821623, 51.31357302830301848, 75.54762311074527759 ) ) ;
#10128 = LINE ( 'NONE', #3830, #16055 ) ;
#10129 = VERTEX_POINT ( 'NONE', #5610 ) ;
#10130 = LINE ( 'NONE', #16610, #3309 ) ;
#10131 = CARTESIAN_POINT ( 'NONE',  ( 30.43948732994507722, 45.16218137147968292, 74.70433879953098710 ) ) ;
#10132 = ORIENTED_EDGE ( 'NONE', *, *, #5168, .T. ) ;
#10133 = CARTESIAN_POINT ( 'NONE',  ( 3.460444912181559474, 49.25145096859824889, 91.74246380123798872 ) ) ;
#10134 = VECTOR ( 'NONE', #5983, 1000.000000000000000 ) ;
#10135 = CARTESIAN_POINT ( 'NONE',  ( 2.027628481303231922, 52.94095516031140392, 77.22796645847455466 ) ) ;
#10136 = EDGE_CURVE ( 'NONE', #880, #19954, #13591, .T. ) ;
#10137 = CARTESIAN_POINT ( 'NONE',  ( -0.9988176903691428077, 49.83852402762217082, 94.39871380123798872 ) ) ;
#10138 = EDGE_CURVE ( 'NONE', #6648, #20749, #17549, .T. ) ;
#10139 = B_SPLINE_CURVE_WITH_KNOTS ( 'NONE', 3,
 ( #14099, #20582, #7923, #4608, #6008, #9533, #4405, #10928, #3136, #2824, #19100, #7716, #9328, #11128, #7820, #14196, #20880, #4511, #20674, #17500, #11029, #4707, #11235, #2924 ),
 .UNSPECIFIED., .F., .F.,
 ( 4, 2, 2, 2, 2, 2, 2, 2, 2, 2, 2, 4 ),
 ( 1.161628372437217770E-05, 0.001362246422599150235, 0.002037561492036547590, 0.002712876561473944945, 0.004063506700348720573, 0.004738821769786108820, 0.005414136839223496200, 0.006764766978098251879, 0.007440082047535629718, 0.008115397116973009292, 0.009466027255847764971, 0.01081665739472252065 ),
 .UNSPECIFIED. ) ;
#10140 = CARTESIAN_POINT ( 'NONE',  ( -4.409036544953043979, 47.67330854490502645, 72.45433879953087342 ) ) ;
#10141 = ORIENTED_EDGE ( 'NONE', *, *, #13298, .T. ) ;
#10142 = DIRECTION ( 'NONE',  ( -0.5813877811927011807, 0.8136266022444372803, 5.636455622144619183E-17 ) ) ;
#10143 = VERTEX_POINT ( 'NONE', #16690 ) ;
#10144 = LINE ( 'NONE', #16625, #16325 ) ;
#10145 = ADVANCED_FACE ( 'NONE', ( #11702 ), #16894, .F. ) ;
#10146 = DIRECTION ( 'NONE',  ( -1.402518428993830937E-16, 1.000000000000000000, -3.469446951953617147E-16 ) ) ;
#10147 = ORIENTED_EDGE ( 'NONE', *, *, #4140, .T. ) ;
#10148 = ADVANCED_FACE ( 'NONE', ( #504 ), #2428, .F. ) ;
#10149 = DIRECTION ( 'NONE',  ( -1.301042606982606060E-16, -1.000000000000000000, 0.000000000000000000 ) ) ;
#10150 = FACE_OUTER_BOUND ( 'NONE', #10111, .T. ) ;
#10151 = VECTOR ( 'NONE', #1665, 1000.000000000000000 ) ;
#10152 = CARTESIAN_POINT ( 'NONE',  ( -4.884656273474451638, 44.39824779480852612, 94.59496379953098710 ) ) ;
#10153 = CARTESIAN_POINT ( 'NONE',  ( 0.5221537403065010796, 44.16218137147968292, 78.25433879953088478 ) ) ;
#10154 = CARTESIAN_POINT ( 'NONE',  ( 0.3419587093557019397, 52.35614670350682331, 78.72223189599347393 ) ) ;
#10155 = VERTEX_POINT ( 'NONE', #18594 ) ;
#10156 = CARTESIAN_POINT ( 'NONE',  ( -4.035110498892168884, 50.97458398355276898, 76.24813767079230331 ) ) ;
#10157 = ORIENTED_EDGE ( 'NONE', *, *, #16170, .T. ) ;
#10158 = CARTESIAN_POINT ( 'NONE',  ( -3.499239294549248758, 37.01553787106989546, 77.72465150895241948 ) ) ;
#10159 = CARTESIAN_POINT ( 'NONE',  ( -6.721687221504229370, 40.35013990712663201, 78.15415281222085753 ) ) ;
#10160 = EDGE_CURVE ( 'NONE', #15424, #15187, #15138, .T. ) ;
#10161 = DIRECTION ( 'NONE',  ( -1.000000000000000000, 0.000000000000000000, 0.000000000000000000 ) ) ;
#10162 = CARTESIAN_POINT ( 'NONE',  ( 5.928963754087452465, 43.92611494815086814, 92.40746379611699979 ) ) ;
#10163 = CARTESIAN_POINT ( 'NONE',  ( 5.666884522201895535, 41.76315400873614436, 93.18871379782397923 ) ) ;
#10164 = CARTESIAN_POINT ( 'NONE',  ( 8.559588968570775336, 45.78687671259945802, 75.44992703482499508 ) ) ;
#10165 = AXIS2_PLACEMENT_3D ( 'NONE', #800, #18666, #900 ) ;
#10166 = ORIENTED_EDGE ( 'NONE', *, *, #9901, .F. ) ;
#10167 = DIRECTION ( 'NONE',  ( 1.540237394707284220E-16, 1.793354297423764243E-16, -1.000000000000000000 ) ) ;
#10168 = DIRECTION ( 'NONE',  ( -0.5813877811927011807, 0.8136266022444372803, 5.636455622144619183E-17 ) ) ;
#10169 = ORIENTED_EDGE ( 'NONE', *, *, #16165, .T. ) ;
#10170 = B_SPLINE_CURVE_WITH_KNOTS ( 'NONE', 3,
 ( #10763, #17227, #11254, #14322, #9658, #1457, #4624, #11357, #14531, #17825, #1560 ),
 .UNSPECIFIED., .F., .F.,
 ( 4, 1, 1, 1, 1, 1, 1, 1, 4 ),
 ( 0.000000000000000000, 0.1077815449370134182, 0.2006545494464173907, 0.2847368448845932765, 0.3681045469499393263, 0.4695596479522798350, 0.6076740370479670750, 0.7836404280850621795, 1.000000000000000000 ),
 .UNSPECIFIED. ) ;
#10171 = CARTESIAN_POINT ( 'NONE',  ( -4.244029479098209379, 50.83477438462418974, 75.97198585835440099 ) ) ;
#10172 = CARTESIAN_POINT ( 'NONE',  ( -3.943187491250720544, 40.73580453397070755, 96.58621379953099506 ) ) ;
#10173 = CARTESIAN_POINT ( 'NONE',  ( -3.943187491250720544, 40.73580453397070755, 94.08621379953100927 ) ) ;
#10174 = EDGE_LOOP ( 'NONE', ( #16883, #15790, #20152, #16266 ) ) ;
#10175 = CARTESIAN_POINT ( 'NONE',  ( -5.154188915835984375, 42.64120994080404614, 96.11746380123797451 ) ) ;
#10176 = CARTESIAN_POINT ( 'NONE',  ( -5.325372805274120047, 38.47710556906300639, 75.75097338717934292 ) ) ;
#10177 = ORIENTED_EDGE ( 'NONE', *, *, #17821, .T. ) ;
#10178 = CARTESIAN_POINT ( 'NONE',  ( 0.5221537403065005245, 44.16218137147968292, 82.45433879953087342 ) ) ;
#10179 = DIRECTION ( 'NONE',  ( 4.818676322157797375E-16, 1.000000000000000000, -0.000000000000000000 ) ) ;
#10180 = ADVANCED_FACE ( 'NONE', ( #10323 ), #2212, .T. ) ;
#10181 = ORIENTED_EDGE ( 'NONE', *, *, #14151, .T. ) ;
#10182 = DIRECTION ( 'NONE',  ( -1.000000000000000000, 0.000000000000000000, 0.000000000000000000 ) ) ;
#10183 = AXIS2_PLACEMENT_3D ( 'NONE', #9441, #15927, #1455 ) ;
#10184 = CARTESIAN_POINT ( 'NONE',  ( -2.416137431568557314, 39.07291177436112406, 93.77371380123797451 ) ) ;
#10185 = ORIENTED_EDGE ( 'NONE', *, *, #19385, .F. ) ;
#10186 = CARTESIAN_POINT ( 'NONE',  ( -4.612897897929109980, 51.30863369456805145, 75.97269380145769446 ) ) ;
#10187 = CARTESIAN_POINT ( 'NONE',  ( 2.118846216502994650, 52.81611540061026489, 76.39834847206340385 ) ) ;
#10188 = EDGE_CURVE ( 'NONE', #880, #6384, #20951, .T. ) ;
#10189 = ADVANCED_FACE ( 'NONE', ( #14021 ), #4114, .F. ) ;
#10190 = CARTESIAN_POINT ( 'NONE',  ( 0.000000000000000000, 0.000000000000000000, 0.000000000000000000 ) ) ;
#10191 = CARTESIAN_POINT ( 'NONE',  ( 5.881110887899452244, 50.21931725652056855, 75.43719735689487038 ) ) ;
#10192 = CARTESIAN_POINT ( 'NONE',  ( 5.570062599089864896, 50.62428647915746183, 77.12188467626378952 ) ) ;
#10193 = VECTOR ( 'NONE', #10680, 1000.000000000000000 ) ;
#10194 = CARTESIAN_POINT ( 'NONE',  ( 11.22215374030649926, 42.96218137147968008, 77.40433879953098995 ) ) ;
#10195 = VERTEX_POINT ( 'NONE', #9249 ) ;
#10196 = EDGE_CURVE ( 'NONE', #6954, #10817, #1929, .T. ) ;
#10197 = CARTESIAN_POINT ( 'NONE',  ( 4.394792124162911762, 36.11365475671116343, 76.60595702694484999 ) ) ;
#10198 = AXIS2_PLACEMENT_3D ( 'NONE', #19974, #10337, #15323 ) ;
#10199 = B_SPLINE_CURVE_WITH_KNOTS ( 'NONE', 3,
 ( #15253, #8876, #668, #10592, #4064, #11961, #18438, #20335, #5562, #10700 ),
 .UNSPECIFIED., .F., .F.,
 ( 4, 2, 2, 2, 4 ),
 ( 0.000000000000000000, 0.0001322853537232420470, 0.0002645707074464840941, 0.0003968560611697261411, 0.0005291414148929681881 ),
 .UNSPECIFIED. ) ;
#10200 = CARTESIAN_POINT ( 'NONE',  ( 8.385679600361122255, 39.92613824206362949, 77.69330938776616335 ) ) ;
#10201 = ORIENTED_EDGE ( 'NONE', *, *, #3112, .F. ) ;
#10202 = DIRECTION ( 'NONE',  ( -0.7071067811865535679, 1.203855704449247279E-16, -0.7071067811865414665 ) ) ;
#10203 = FACE_OUTER_BOUND ( 'NONE', #11516, .T. ) ;
#10204 = CARTESIAN_POINT ( 'NONE',  ( -7.202537930885374529, 41.41097462079392955, 78.61536821129558916 ) ) ;
#10205 = ORIENTED_EDGE ( 'NONE', *, *, #17583, .T. ) ;
#10206 = VERTEX_POINT ( 'NONE', #1361 ) ;
#10207 = AXIS2_PLACEMENT_3D ( 'NONE', #18959, #20647, #5978 ) ;
#10208 = CLOSED_SHELL ( 'NONE', ( #3508, #19874, #10189, #17792, #7646, #3642, #20423, #13505, #4029, #18308, #95, #151, #19867, #10148, #4765, #18160, #12508, #770, #20448, #3492, #8074, #5710, #3725, #3611, #20053, #16542, #76, #15573, #16228, #11031, #9632 ) ) ;
#10209 = CARTESIAN_POINT ( 'NONE',  ( 6.470644262523409296, 49.79467064229719853, 78.73390793106847241 ) ) ;
#10210 = VERTEX_POINT ( 'NONE', #12432 ) ;
#10211 = CARTESIAN_POINT ( 'NONE',  ( 27.27315414062681853, 40.36218137147969287, 87.85433879953103542 ) ) ;
#10212 = CARTESIAN_POINT ( 'NONE',  ( 8.887668352622405621, 41.43063037816333605, 75.36022115247205022 ) ) ;
#10213 = CARTESIAN_POINT ( 'NONE',  ( -2.985824661004252700, 51.57396771150768444, 78.81127817498905586 ) ) ;
#10214 = CARTESIAN_POINT ( 'NONE',  ( 8.362036131964948993, 41.75873031979976702, 77.44666563814885762 ) ) ;
#10215 = FACE_OUTER_BOUND ( 'NONE', #2622, .T. ) ;
#10216 = CIRCLE ( 'NONE', #1027, 0.5999999999999998668 ) ;
#10217 = FACE_OUTER_BOUND ( 'NONE', #5243, .T. ) ;
#10218 = CIRCLE ( 'NONE', #6105, 4.000000000000000000 ) ;
#10219 = CARTESIAN_POINT ( 'NONE',  ( 8.119551934336415755, 43.80226376792169418, 75.45433879953087342 ) ) ;
#10220 = DIRECTION ( 'NONE',  ( -1.000000000000000000, -1.402518428993831676E-16, -1.196361017915039239E-16 ) ) ;
#10221 = CARTESIAN_POINT ( 'NONE',  ( 3.460444912181559474, 49.25145096859824889, 92.99246380123798872 ) ) ;
#10222 = VECTOR ( 'NONE', #9386, 1000.000000000000000 ) ;
#10223 = CARTESIAN_POINT ( 'NONE',  ( 2.722153740306499703, 47.73989013547934945, 54.55433879953099563 ) ) ;
#10224 = ORIENTED_EDGE ( 'NONE', *, *, #6633, .T. ) ;
#10225 = CARTESIAN_POINT ( 'NONE',  ( 0.5705749803268341802, 52.35434406645455141, 75.97198585835440099 ) ) ;
#10226 = VERTEX_POINT ( 'NONE', #931 ) ;
#10227 = CARTESIAN_POINT ( 'NONE',  ( 5.363562441227258226, 50.78054159302179471, 77.28832336276830972 ) ) ;
#10228 = DIRECTION ( 'NONE',  ( 1.540237394707284220E-16, 1.793354297423764243E-16, -1.000000000000000000 ) ) ;
#10229 = CARTESIAN_POINT ( 'NONE',  ( -4.392776879941215462, 37.60686397218470489, 78.93508260432024315 ) ) ;
#10230 = CARTESIAN_POINT ( 'NONE',  ( -2.416137431568557314, 39.07291177436112406, 93.77371380123797451 ) ) ;
#10231 = AXIS2_PLACEMENT_3D ( 'NONE', #8692, #10082, #19841 ) ;
#10232 = CARTESIAN_POINT ( 'NONE',  ( -4.766817752550178255, 37.12851695549264974, 75.97348137399042400 ) ) ;
#10233 = CARTESIAN_POINT ( 'NONE',  ( 13.72215374030650104, 51.36218137147968577, 95.05433879953098142 ) ) ;
#10234 = CARTESIAN_POINT ( 'NONE',  ( 5.540944419992344550, 50.64230199400775945, 78.19629421043239859 ) ) ;
#10235 = ORIENTED_EDGE ( 'NONE', *, *, #13895, .T. ) ;
#10236 = ORIENTED_EDGE ( 'NONE', *, *, #3514, .T. ) ;
#10237 = AXIS2_PLACEMENT_3D ( 'NONE', #9484, #15971, #12872 ) ;
#10238 = CARTESIAN_POINT ( 'NONE',  ( 9.092498755203211047, 42.04452008889646208, 79.47377622490290605 ) ) ;
#10239 = CARTESIAN_POINT ( 'NONE',  ( 13.32277635493562329, 51.36218137147968577, 54.55433879953099563 ) ) ;
#10240 = DIRECTION ( 'NONE',  ( 1.000000000000000000, -4.930380657631323784E-32, 3.893792155548169402E-16 ) ) ;
#10241 = EDGE_LOOP ( 'NONE', ( #17937, #20226, #4031, #11862 ) ) ;
#10242 =( REPRESENTATION_RELATIONSHIP ('NONE','NONE', #11365, #9739 ) REPRESENTATION_RELATIONSHIP_WITH_TRANSFORMATION ( #14101 )SHAPE_REPRESENTATION_RELATIONSHIP( ) );
#10243 = CARTESIAN_POINT ( 'NONE',  ( -4.813079231556614879, 45.05781033453988016, 95.05433879953105247 ) ) ;
#10244 = CARTESIAN_POINT ( 'NONE',  ( 1.652727357819364640, 35.35299279957455809, 75.45433879953087342 ) ) ;
#10245 = CARTESIAN_POINT ( 'NONE',  ( -5.058133621542618030, 44.89684013992257405, 91.74246380294499659 ) ) ;
#10246 = CARTESIAN_POINT ( 'NONE',  ( -7.203585122226456861, 41.42633110391964379, 78.75487387812985673 ) ) ;
#10247 = EDGE_CURVE ( 'NONE', #17173, #15408, #11597, .T. ) ;
#10248 = CARTESIAN_POINT ( 'NONE',  ( -4.567115856812060670, 47.10047254335474065, 90.96121380123797451 ) ) ;
#10249 = B_SPLINE_SURFACE_WITH_KNOTS ( 'NONE', 3, 1, ( 
 ( #18056, #6346 ),
 ( #79, #11162 ),
 ( #13167, #19326 ),
 ( #11271, #1682 ),
 ( #3175, #17630 ),
 ( #8164, #14858 ),
 ( #9678, #6663 ),
 ( #9883, #180 ),
 ( #6247, #11475 ),
 ( #6560, #3067 ),
 ( #1794, #21016 ) ),
 .UNSPECIFIED., .F., .F., .F.,
 ( 4, 1, 1, 1, 1, 1, 1, 1, 4 ),
 ( 2, 2 ),
 ( 0.000000000000000000, 0.1088348533325064621, 0.2165694074861221896, 0.3273827587112763671, 0.4434819477562966239, 0.5673092549448471855, 0.7000542417988985244, 0.8441436218123770097, 1.000000000000000000 ),
 ( 0.000000000000000000, 1.000000000000000000 ),
 .UNSPECIFIED. ) ;
#10250 = UNCERTAINTY_MEASURE_WITH_UNIT (LENGTH_MEASURE( 1.000000000000000082E-05 ), #10286, 'distance_accuracy_value', 'NONE');
#10251 = LINE ( 'NONE', #13740, #15340 ) ;
#10252 = EDGE_LOOP ( 'NONE', ( #17838, #7965, #569, #8046, #14431, #6377, #2264, #8367, #14635, #7841, #13743, #9150, #13556, #2473, #11869, #14748, #7151, #691, #10492, #16789, #2567, #9390, #11555, #8981 ) ) ;
#10253 = CARTESIAN_POINT ( 'NONE',  ( 0.5221537403065104055, 40.36218137147969998, 46.15433879953098284 ) ) ;
#10254 = EDGE_LOOP ( 'NONE', ( #19938, #13936, #12551, #2785 ) ) ;
#10255 = AXIS2_PLACEMENT_3D ( 'NONE', #18311, #3733, #11526 ) ;
#10256 = CARTESIAN_POINT ( 'NONE',  ( -0.4699484075729999377, 51.36218137147968577, 87.21440135111343750 ) ) ;
#10257 = VECTOR ( 'NONE', #17042, 1000.000000000000000 ) ;
#10258 = CARTESIAN_POINT ( 'NONE',  ( -3.350035803220276609, 49.20851703305431357, 90.72683880123797451 ) ) ;
#10259 = ORIENTED_EDGE ( 'NONE', *, *, #12611, .F. ) ;
#10260 = LINE ( 'NONE', #16735, #11004 ) ;
#10261 = CARTESIAN_POINT ( 'NONE',  ( 5.722153740306498371, 44.16218137147968292, 94.58161078214052964 ) ) ;
#10262 = EDGE_CURVE ( 'NONE', #20901, #3734, #7418, .T. ) ;
#10263 = CARTESIAN_POINT ( 'NONE',  ( -3.778837258911088792, 51.90462289030131160, 79.34012906335151172 ) ) ;
#10264 = DIRECTION ( 'NONE',  ( 1.290716872006552287E-16, 1.000000000000000000, 0.000000000000000000 ) ) ;
#10265 = CARTESIAN_POINT ( 'NONE',  ( 0.3504751631991869787, 52.35607954813841758, 78.76353264627590534 ) ) ;
#10266 = ORIENTED_EDGE ( 'NONE', *, *, #2365, .T. ) ;
#10267 = CARTESIAN_POINT ( 'NONE',  ( 31.07218010054375412, 42.76218137147968434, 64.80574467885102763 ) ) ;
#10268 = ORIENTED_EDGE ( 'NONE', *, *, #13092, .T. ) ;
#10269 = CARTESIAN_POINT ( 'NONE',  ( -3.243516849062964891, 36.87779780655007045, 77.90799200028293114 ) ) ;
#10270 = CARTESIAN_POINT ( 'NONE',  ( -7.736834117765939212, 41.07628627713002345, 76.72474157890661672 ) ) ;
#10271 = EDGE_CURVE ( 'NONE', #12203, #10073, #13635, .T. ) ;
#10272 = CARTESIAN_POINT ( 'NONE',  ( -4.163054115940463262, 37.43240098938879612, 77.00485536016182664 ) ) ;
#10273 = CARTESIAN_POINT ( 'NONE',  ( 6.921466148593897749, 50.37568168049836714, 78.61296362383696135 ) ) ;
#10274 = VECTOR ( 'NONE', #13133, 1000.000000000000000 ) ;
#10275 = CARTESIAN_POINT ( 'NONE',  ( 0.2541436421823717318, 38.02374091943176637, 91.70433879782397923 ) ) ;
#10276 = CARTESIAN_POINT ( 'NONE',  ( 33.61275266354798674, 36.96218137147968719, 93.55433879953098142 ) ) ;
#10277 = ORIENTED_EDGE ( 'NONE', *, *, #19848, .T. ) ;
#10278 = CARTESIAN_POINT ( 'NONE',  ( 23.03948732994508575, 43.16218137147968292, 76.90433879953101837 ) ) ;
#10279 = B_SPLINE_CURVE_WITH_KNOTS ( 'NONE', 3,
 ( #12736, #9346, #7845, #2738, #6134, #14328, #20806, #18805, #15729, #19119, #1147, #2941, #7525, #13904, #926, #10743 ),
 .UNSPECIFIED., .F., .F.,
 ( 4, 2, 2, 2, 2, 2, 2, 4 ),
 ( 0.000000000000000000, 0.0002950570430945601377, 0.0005901140861891202754, 0.0008851711292836804672, 0.001180228172378240551, 0.001770342258567334046, 0.002065399301661875915, 0.002360456344756417784 ),
 .UNSPECIFIED. ) ;
#10280 = ORIENTED_EDGE ( 'NONE', *, *, #3782, .F. ) ;
#10281 = DIRECTION ( 'NONE',  ( 0.000000000000000000, -2.168404344970984808E-15, -1.000000000000000000 ) ) ;
#10282 = CARTESIAN_POINT ( 'NONE',  ( -0.8237052942265477018, 49.18499566818285018, 93.69558879953099506 ) ) ;
#10283 = CARTESIAN_POINT ( 'NONE',  ( -2.077846259693550746, 39.65884927180063357, 95.41433879953098085 ) ) ;
#10284 = CARTESIAN_POINT ( 'NONE',  ( -7.474360244459849589, 42.69441725426494827, 76.61471288230795551 ) ) ;
#10285 = VERTEX_POINT ( 'NONE', #7954 ) ;
#10286 =( LENGTH_UNIT ( ) NAMED_UNIT ( * ) SI_UNIT ( .MILLI., .METRE. ) );
#10287 = DIRECTION ( 'NONE',  ( -0.000000000000000000, 1.000000000000000000, -0.000000000000000000 ) ) ;
#10288 = VERTEX_POINT ( 'NONE', #6658 ) ;
#10289 = VECTOR ( 'NONE', #10085, 1000.000000000000000 ) ;
#10290 = CARTESIAN_POINT ( 'NONE',  ( 1.656782470118943751, 39.12201036244813679, 95.05433879953095300 ) ) ;
#10291 = LINE ( 'NONE', #14640, #16637 ) ;
#10292 = VECTOR ( 'NONE', #13511, 1000.000000000000000 ) ;
#10293 = ORIENTED_EDGE ( 'NONE', *, *, #9073, .F. ) ;
#10294 = CARTESIAN_POINT ( 'NONE',  ( -4.147124323215474639, 37.44553550079235293, 78.31852111096432623 ) ) ;
#10295 = CARTESIAN_POINT ( 'NONE',  ( -0.9988176903691428077, 49.83852402762217082, 95.80496380123798872 ) ) ;
#10296 = EDGE_LOOP ( 'NONE', ( #10951, #13827, #19745, #10002 ) ) ;
#10297 = CARTESIAN_POINT ( 'NONE',  ( -3.777846259693487863, 51.36218137147968577, 53.35433879953099989 ) ) ;
#10298 = DIRECTION ( 'NONE',  ( 1.000000000000000000, 0.000000000000000000, 0.000000000000000000 ) ) ;
#10299 = CARTESIAN_POINT ( 'NONE',  ( -5.784195910403845176, 44.99242805365518194, 90.88308880123798872 ) ) ;
#10300 = DIRECTION ( 'NONE',  ( -0.1823574043109634224, -0.9832323108467134753, -3.584394978051716837E-16 ) ) ;
#10301 = CARTESIAN_POINT ( 'NONE',  ( 5.859131993956401274, 51.16038512709904040, 75.36137945677606353 ) ) ;
#10303 = ADVANCED_FACE ( 'NONE', ( #6240 ), #4849, .F. ) ;
#10302 = DIRECTION ( 'NONE',  ( -1.110223024625156540E-16, -1.000000000000000000, -5.922860397471808077E-17 ) ) ;
#10304 = AXIS2_PLACEMENT_3D ( 'NONE', #8635, #3924, #2337 ) ;
#10305 = DIRECTION ( 'NONE',  ( -1.000000000000000000, 0.000000000000000000, 0.000000000000000000 ) ) ;
#10306 = VECTOR ( 'NONE', #7135, 1000.000000000000000 ) ;
#10307 = VERTEX_POINT ( 'NONE', #14436 ) ;
#10308 = EDGE_CURVE ( 'NONE', #14607, #11193, #6444, .T. ) ;
#10309 = DIRECTION ( 'NONE',  ( -0.3165065846431826535, -0.9485903129789527988, 0.000000000000000000 ) ) ;
#10310 = ORIENTED_EDGE ( 'NONE', *, *, #11997, .T. ) ;
#10311 = CARTESIAN_POINT ( 'NONE',  ( -4.523565618882782857, 37.69517167404197266, 75.36122732895108811 ) ) ;
#10312 = EDGE_CURVE ( 'NONE', #6327, #16992, #1570, .T. ) ;
#10313 = CARTESIAN_POINT ( 'NONE',  ( -1.477846259693499364, 49.81903562097207327, 83.21119304902337888 ) ) ;
#10314 = CARTESIAN_POINT ( 'NONE',  ( -0.9988176903691428077, 49.83852402762217082, 94.55496380123798872 ) ) ;
#10315 = EDGE_LOOP ( 'NONE', ( #4344, #20408, #15930, #13192 ) ) ;
#10316 = EDGE_CURVE ( 'NONE', #8610, #2109, #14338, .T. ) ;
#10317 = CARTESIAN_POINT ( 'NONE',  ( 6.448646529778700121, 49.81091948135299674, 78.84682786933051091 ) ) ;
#10318 = ORIENTED_EDGE ( 'NONE', *, *, #5060, .F. ) ;
#10319 = EDGE_CURVE ( 'NONE', #9753, #10288, #18421, .T. ) ;
#10320 = CARTESIAN_POINT ( 'NONE',  ( -3.607485548685017029, 36.27216495724725576, 77.44024473021482891 ) ) ;
#10321 = CARTESIAN_POINT ( 'NONE',  ( -0.1389469955404790957, 52.97235366542109603, 75.45826338387253429 ) ) ;
#10322 = VECTOR ( 'NONE', #18414, 1000.000000000000000 ) ;
#10323 = FACE_OUTER_BOUND ( 'NONE', #20662, .T. ) ;
#10324 = CARTESIAN_POINT ( 'NONE',  ( 4.540095451430588902, 52.13470428702989068, 76.74217282813371810 ) ) ;
#10325 = FACE_OUTER_BOUND ( 'NONE', #14183, .T. ) ;
#10326 = CARTESIAN_POINT ( 'NONE',  ( 3.460444912181559474, 49.25145096859824889, 95.64871380123798872 ) ) ;
#10327 = CARTESIAN_POINT ( 'NONE',  ( 8.794665453373390562, 41.15189478912013499, 76.14505377247542128 ) ) ;
#10328 = CARTESIAN_POINT ( 'NONE',  ( -0.8448747701364694995, 38.43386606678133433, 92.55433879953096721 ) ) ;
#10329 = CARTESIAN_POINT ( 'NONE',  ( 4.098701607150998072, 51.53591119238402740, 76.47586842453881673 ) ) ;
#10330 = CARTESIAN_POINT ( 'NONE',  ( 5.180932498246527018, 37.42231731781541271, 77.73906448345020692 ) ) ;
#10331 = CARTESIAN_POINT ( 'NONE',  ( -2.904223097202481174, 48.62752260303690122, 95.33621380294498238 ) ) ;
#10332 = CARTESIAN_POINT ( 'NONE',  ( 8.352500096663396434, 41.72785666267516547, 76.03373457610489083 ) ) ;
#10333 = VERTEX_POINT ( 'NONE', #1674 ) ;
#10334 = CARTESIAN_POINT ( 'NONE',  ( 2.522153740306509739, 49.16218137147969003, 58.55433879953100984 ) ) ;
#10335 = AXIS2_PLACEMENT_3D ( 'NONE', #2117, #4117, #20283 ) ;
#10336 = ORIENTED_EDGE ( 'NONE', *, *, #4422, .T. ) ;
#10337 = DIRECTION ( 'NONE',  ( -1.779391786395883536E-16, -5.922860397471806844E-17, 1.000000000000000000 ) ) ;
#10338 = DIRECTION ( 'NONE',  ( -1.193617070626243484E-16, -1.000000000000000000, 0.000000000000000000 ) ) ;
#10339 = EDGE_CURVE ( 'NONE', #20669, #11820, #12743, .T. ) ;
#10340 = DIRECTION ( 'NONE',  ( -1.540237394707284467E-16, -1.793354297423764243E-16, 1.000000000000000000 ) ) ;
#10341 = CARTESIAN_POINT ( 'NONE',  ( -3.350035803220276609, 49.20851703305431357, 95.88308880123798872 ) ) ;
#10342 = LINE ( 'NONE', #13612, #20404 ) ;
#10343 = CARTESIAN_POINT ( 'NONE',  ( 28.43948732994508077, 45.16218137147969003, 76.90433879953101837 ) ) ;
#10344 = FACE_OUTER_BOUND ( 'NONE', #8867, .T. ) ;
#10345 = CARTESIAN_POINT ( 'NONE',  ( -0.9504375969237850441, 51.37401713635502887, 77.77566232894263010 ) ) ;
#10346 = VERTEX_POINT ( 'NONE', #8158 ) ;
#10347 = ORIENTED_EDGE ( 'NONE', *, *, #18419, .F. ) ;
#10348 = B_SPLINE_CURVE_WITH_KNOTS ( 'NONE', 3,
 ( #16357, #18050, #19534, #3473, #74, #17736, #3057, #9564, #19219, #4636 ),
 .UNSPECIFIED., .F., .F.,
 ( 4, 2, 2, 2, 4 ),
 ( 0.000000000000000000, 0.0001230208117932171999, 0.0002460416235864343998, 0.0003690624353796515726, 0.0004920832471728687997 ),
 .UNSPECIFIED. ) ;
#10349 = CARTESIAN_POINT ( 'NONE',  ( 8.872773925109784798, 41.38599083402314704, 79.54845644658969661 ) ) ;
#10350 = CARTESIAN_POINT ( 'NONE',  ( 5.453344025566023490, 40.65105419805430387, 72.45433879953087342 ) ) ;
#10351 = FACE_BOUND ( 'NONE', #1209, .T. ) ;
#10352 = ORIENTED_EDGE ( 'NONE', *, *, #12787, .F. ) ;
#10353 = DIRECTION ( 'NONE',  ( -1.000000000000000000, 1.110223024625156540E-16, -1.779391786395883043E-16 ) ) ;
#10354 = DIRECTION ( 'NONE',  ( -3.211742425186504723E-16, 5.922860397471811774E-17, -1.000000000000000000 ) ) ;
#10355 = CIRCLE ( 'NONE', #2174, 1.399999999999995026 ) ;
#10356 = CARTESIAN_POINT ( 'NONE',  ( -8.192078482032012943, 42.93655631659661509, 75.45433879953087342 ) ) ;
#10357 = CARTESIAN_POINT ( 'NONE',  ( 4.001626195812781006, 40.29782224849783745, 89.72723091094957226 ) ) ;
#10358 = CARTESIAN_POINT ( 'NONE',  ( 1.965820793441009240, 52.94144253664489241, 77.13040333250513925 ) ) ;
#10359 = CARTESIAN_POINT ( 'NONE',  ( -3.584565806390786591, 36.25523506687804343, 78.05869123030269918 ) ) ;
#10360 = CARTESIAN_POINT ( 'NONE',  ( -5.784195910403845176, 44.99242805365518194, 93.38308880123798872 ) ) ;
#10361 = B_SPLINE_CURVE_WITH_KNOTS ( 'NONE', 3,
 ( #13181, #19340, #3383, #4971 ),
 .UNSPECIFIED., .F., .F.,
 ( 4, 4 ),
 ( 2.201117333616983738E-17, 0.002523081261280070431 ),
 .UNSPECIFIED. ) ;
#10362 = CARTESIAN_POINT ( 'NONE',  ( 0.3279640439667353413, 52.35988168082470651, 72.45433879953087342 ) ) ;
#10363 = ORIENTED_EDGE ( 'NONE', *, *, #7748, .F. ) ;
#10364 = CARTESIAN_POINT ( 'NONE',  ( -1.769308508470985419, 51.40850462968639079, 72.45432679953087529 ) ) ;
#10365 = ORIENTED_EDGE ( 'NONE', *, *, #7274, .T. ) ;
#10366 = PLANE ( 'NONE',  #14274 ) ;
#10367 = CARTESIAN_POINT ( 'NONE',  ( -5.784195910403845176, 44.99242805365518194, 90.88308880123798872 ) ) ;
#10368 = ORIENTED_EDGE ( 'NONE', *, *, #17583, .F. ) ;
#10369 = CARTESIAN_POINT ( 'NONE',  ( 6.880132251722071324, 48.33664052787082710, 72.45433879953087342 ) ) ;
#10370 = CARTESIAN_POINT ( 'NONE',  ( -3.134114116279072881, 48.15229756555780227, 94.43871379953097289 ) ) ;
#10371 = CARTESIAN_POINT ( 'NONE',  ( -3.512376142844359173, 52.09502624807847582, 79.07098488719154261 ) ) ;
#10372 = CARTESIAN_POINT ( 'NONE',  ( 0.8304091259513172174, 52.95680132091538894, 77.54407394899503458 ) ) ;
#10373 = CARTESIAN_POINT ( 'NONE',  ( 0.8496841725525090538, 52.96357321910183913, 76.36683753262285279 ) ) ;
#10374 = FACE_OUTER_BOUND ( 'NONE', #3323, .T. ) ;
#10375 = ORIENTED_EDGE ( 'NONE', *, *, #7512, .F. ) ;
#10376 = CARTESIAN_POINT ( 'NONE',  ( 0.5221537403064990812, 44.16218137147969003, 95.05433879953096721 ) ) ;
#10377 = EDGE_CURVE ( 'NONE', #14607, #6086, #20812, .T. ) ;
#10378 = ORIENTED_EDGE ( 'NONE', *, *, #17215, .T. ) ;
#10379 = ADVANCED_BREP_SHAPE_REPRESENTATION ( '', ( #4605, #18366 ), #7495 ) ;
#10380 = CARTESIAN_POINT ( 'NONE',  ( 8.872773925109784798, 41.38599083402314704, 79.54845644658969661 ) ) ;
#10381 = DIRECTION ( 'NONE',  ( -1.540237394707284220E-16, -1.793354297423764243E-16, 1.000000000000000000 ) ) ;
#10382 = CARTESIAN_POINT ( 'NONE',  ( 0.2012661975153932636, 37.99231409082479161, 92.61876351041186695 ) ) ;
#10383 = CARTESIAN_POINT ( 'NONE',  ( 5.467491823421675612, 37.62122069371999800, 76.05323035213213245 ) ) ;
#10384 = CARTESIAN_POINT ( 'NONE',  ( 2.463659247115866258, 38.82793883177424732, 94.12621379782399345 ) ) ;
#10385 = DIRECTION ( 'NONE',  ( 0.02533578529877749883, 0.9996789974703350623, 1.831801750099157041E-16 ) ) ;
#10386 = EDGE_CURVE ( 'NONE', #4065, #13955, #10348, .T. ) ;
#10387 = ORIENTED_EDGE ( 'NONE', *, *, #12369, .F. ) ;
#10388 = CARTESIAN_POINT ( 'NONE',  ( 8.788342534296722519, 41.13294459952883386, 78.64407474691132904 ) ) ;
#10389 = ORIENTED_EDGE ( 'NONE', *, *, #7380, .F. ) ;
#10390 = DIRECTION ( 'NONE',  ( 1.000000000000000000, 1.402518428993831183E-16, -4.344610079045915326E-32 ) ) ;
#10391 = CARTESIAN_POINT ( 'NONE',  ( -2.904223097202481174, 48.62752260303690122, 95.02371379953099506 ) ) ;
#10392 = CARTESIAN_POINT ( 'NONE',  ( 6.102441102155617969, 43.42752260303680600, 94.55496379953098085 ) ) ;
#10393 = CARTESIAN_POINT ( 'NONE',  ( -8.102959993061887189, 42.23164920826034319, 76.93555611204594413 ) ) ;
#10394 = ORIENTED_EDGE ( 'NONE', *, *, #191, .T. ) ;
#10395 = FILL_AREA_STYLE_COLOUR ( '', #19717 ) ;
#10396 = DIRECTION ( 'NONE',  ( -1.540237394707284467E-16, -1.793354297423764243E-16, 1.000000000000000000 ) ) ;
#10397 = EDGE_LOOP ( 'NONE', ( #18797, #18019, #11532, #9352 ) ) ;
#10398 = PLANE ( 'NONE',  #10510 ) ;
#10399 = LINE ( 'NONE', #7175, #8139 ) ;
#10400 = ORIENTED_EDGE ( 'NONE', *, *, #10656, .T. ) ;
#10401 = LINE ( 'NONE', #10618, #20388 ) ;
#10402 = CARTESIAN_POINT ( 'NONE',  ( -5.784195910403845176, 44.99242805365518194, 94.78933880123798872 ) ) ;
#10403 = EDGE_CURVE ( 'NONE', #18369, #2200, #7100, .T. ) ;
#10404 = ORIENTED_EDGE ( 'NONE', *, *, #18450, .T. ) ;
#10405 = CARTESIAN_POINT ( 'NONE',  ( -4.783040473602117260, 51.18705603930939674, 76.11505395997643575 ) ) ;
#10406 = CYLINDRICAL_SURFACE ( 'NONE', #19026, 6.200000000000000178 ) ;
#10407 = CARTESIAN_POINT ( 'NONE',  ( 6.198496396448986090, 45.68315280215533392, 90.33621380123798872 ) ) ;
#10408 = CARTESIAN_POINT ( 'NONE',  ( -4.735411308350331083, 37.10531828029095891, 75.97251605650340878 ) ) ;
#10409 = CARTESIAN_POINT ( 'NONE',  ( 5.053692675489761754, 42.04909006277621586, 93.89183879953097289 ) ) ;
#10410 = CARTESIAN_POINT ( 'NONE',  ( -4.454500421143473332, 37.64505674804929924, 79.54845644658969661 ) ) ;
#10411 = EDGE_CURVE ( 'NONE', #4997, #3547, #16047, .T. ) ;
#10412 = ORIENTED_EDGE ( 'NONE', *, *, #8155, .T. ) ;
#10413 = ORIENTED_EDGE ( 'NONE', *, *, #2870, .T. ) ;
#10414 = CARTESIAN_POINT ( 'NONE',  ( 0.8535366408858915399, 52.96430285769372404, 75.36710396340995999 ) ) ;
#10415 = EDGE_CURVE ( 'NONE', #14613, #6086, #4736, .T. ) ;
#10416 = VERTEX_POINT ( 'NONE', #11679 ) ;
#10417 = DIRECTION ( 'NONE',  ( 1.540237394707284220E-16, 1.793354297423764243E-16, -1.000000000000000000 ) ) ;
#10418 = CARTESIAN_POINT ( 'NONE',  ( 8.527988662190095326, 48.03182059810101379, 79.44551527011911674 ) ) ;
#10419 = CARTESIAN_POINT ( 'NONE',  ( 6.828503391016846891, 43.33193468930419101, 95.41433880123797451 ) ) ;
#10420 = VERTEX_POINT ( 'NONE', #10297 ) ;
#10421 = CARTESIAN_POINT ( 'NONE',  ( 2.108290839596759003, 51.34989793853182505, 77.84551527011910821 ) ) ;
#10422 = ORIENTED_EDGE ( 'NONE', *, *, #3250, .T. ) ;
#10423 = CARTESIAN_POINT ( 'NONE',  ( 11.22215374030649926, 42.76218137147968434, 80.55433879953099563 ) ) ;
#10424 = EDGE_CURVE ( 'NONE', #1387, #10593, #2088, .T. ) ;
#10425 = FACE_OUTER_BOUND ( 'NONE', #2543, .T. ) ;
#10426 = CARTESIAN_POINT ( 'NONE',  ( 8.550070540977731781, 40.41882831985841307, 75.56834740413086138 ) ) ;
#10427 = DIRECTION ( 'NONE',  ( 1.000000000000000000, 0.000000000000000000, 0.000000000000000000 ) ) ;
#10429 = EDGE_CURVE ( 'NONE', #18295, #7860, #410, .T. ) ;
#10428 = CARTESIAN_POINT ( 'NONE',  ( -3.104272635537439928, 51.51688312651948820, 79.08698131281367694 ) ) ;
#10430 = DIRECTION ( 'NONE',  ( 0.000000000000000000, 0.000000000000000000, 1.000000000000000000 ) ) ;
#10431 = CARTESIAN_POINT ( 'NONE',  ( -5.784195910403845176, 44.99242805365518194, 94.78933880123798872 ) ) ;
#10432 = PRODUCT_DEFINITION_SHAPE ( 'NONE', 'NONE',  #21035 ) ;
#10433 = CARTESIAN_POINT ( 'NONE',  ( 8.225112643453085681, 41.36496456502055707, 76.07953452682116335 ) ) ;
#10434 = CARTESIAN_POINT ( 'NONE',  ( -3.350035803220276609, 49.20851703305431357, 91.97683880123797451 ) ) ;
#10435 = CARTESIAN_POINT ( 'NONE',  ( 1.064787648071129134, 38.29826807256112176, 92.55433879953091036 ) ) ;
#10436 = CARTESIAN_POINT ( 'NONE',  ( 5.197017349930873387, 50.72462959604935406, 75.36146177662637058 ) ) ;
#10437 = ADVANCED_FACE ( 'NONE', ( #11777 ), #9203, .T. ) ;
#10438 = CARTESIAN_POINT ( 'NONE',  ( 6.102441102155617969, 43.42752260303680600, 92.36746380294498238 ) ) ;
#10439 = EDGE_CURVE ( 'NONE', #20391, #14499, #8627, .T. ) ;
#10440 = CARTESIAN_POINT ( 'NONE',  ( 8.365153831044532140, 41.76897630594757516, 76.08825944838494593 ) ) ;
#10441 = CARTESIAN_POINT ( 'NONE',  ( 0.3298136261391984014, 52.35624255821358020, 76.26461983994238381 ) ) ;
#10442 = ADVANCED_FACE ( 'NONE', ( #16874 ), #10508, .T. ) ;
#10443 = CYLINDRICAL_SURFACE ( 'NONE', #8820, 8.199999999999995737 ) ;
#10444 = CARTESIAN_POINT ( 'NONE',  ( 5.753005855668248181, 51.23877623043087937, 78.93669174070734584 ) ) ;
#10445 = CARTESIAN_POINT ( 'NONE',  ( 8.385679600361122255, 39.92613824206362949, 77.69330938776616335 ) ) ;
#10446 = CARTESIAN_POINT ( 'NONE',  ( -5.154188915835984375, 42.64120994080404614, 96.11746380123797451 ) ) ;
#10447 = CARTESIAN_POINT ( 'NONE',  ( 2.643026689701002407, 51.46641972551267941, 75.45433879953087342 ) ) ;
#10448 = LINE ( 'NONE', #7003, #5865 ) ;
#10449 = DIRECTION ( 'NONE',  ( -0.3165065846431827090, -0.9485903129789529098, 0.000000000000000000 ) ) ;
#10450 = DIRECTION ( 'NONE',  ( -1.779391786395883536E-16, -5.922860397471806844E-17, 1.000000000000000000 ) ) ;
#10451 = ORIENTED_EDGE ( 'NONE', *, *, #13144, .F. ) ;
#10452 = ORIENTED_EDGE ( 'NONE', *, *, #18480, .T. ) ;
#10453 = CARTESIAN_POINT ( 'NONE',  ( 8.886583547266173611, 41.42737914769194418, 79.54795956895829079 ) ) ;
#10455 = EDGE_CURVE ( 'NONE', #3218, #15454, #5219, .T. ) ;
#10454 = LINE ( 'NONE', #20622, #2647 ) ;
#10456 = CARTESIAN_POINT ( 'NONE',  ( -2.939085670389444793, 51.59587639763223166, 72.45433879953087342 ) ) ;
#10457 = VERTEX_POINT ( 'NONE', #6108 ) ;
#10458 = CARTESIAN_POINT ( 'NONE',  ( -3.430302262420787063, 39.98804081939900357, 95.05433879953099563 ) ) ;
#10459 = VECTOR ( 'NONE', #10053, 1000.000000000000000 ) ;
#10460 = CARTESIAN_POINT ( 'NONE',  ( 0.3821786226492926430, 35.36301154328572949, 76.86610350541323555 ) ) ;
#10461 = CARTESIAN_POINT ( 'NONE',  ( 28.52215374030649642, 44.16218137147969003, 87.85433879953103542 ) ) ;
#10462 = EDGE_CURVE ( 'NONE', #6478, #4231, #8561, .T. ) ;
#10463 = CARTESIAN_POINT ( 'NONE',  ( -0.6028239774188565159, 52.89035653119623959, 79.22266899401112994 ) ) ;
#10464 = CARTESIAN_POINT ( 'NONE',  ( -7.576204955092350701, 47.69026255563115768, 78.31886496287775401 ) ) ;
#10465 = CARTESIAN_POINT ( 'NONE',  ( 3.788215052820487205, 39.19523464621513398, 90.24306233796824017 ) ) ;
#10466 = CARTESIAN_POINT ( 'NONE',  ( -3.279987361312213690, 36.94427024389478476, 77.85659439586764563 ) ) ;
#10467 = DIRECTION ( 'NONE',  ( -0.5813877811927011807, 0.8136266022444372803, 5.636455622144619183E-17 ) ) ;
#10468 = VERTEX_POINT ( 'NONE', #7819 ) ;
#10469 = CARTESIAN_POINT ( 'NONE',  ( 5.568913169576547695, 50.62012213993821064, 77.10005730845655592 ) ) ;
#10470 = ORIENTED_EDGE ( 'NONE', *, *, #19762, .F. ) ;
#10471 = CARTESIAN_POINT ( 'NONE',  ( -4.391572913631113906, 50.71986899290229900, 78.89490084226201816 ) ) ;
#10472 = CARTESIAN_POINT ( 'NONE',  ( -3.943187491250720544, 40.73580453397070755, 95.64871380294496817 ) ) ;
#10473 = ORIENTED_EDGE ( 'NONE', *, *, #14818, .T. ) ;
#10474 = CARTESIAN_POINT ( 'NONE',  ( -4.622577041588896485, 46.56120873422322859, 92.56371379782397923 ) ) ;
#10475 = CARTESIAN_POINT ( 'NONE',  ( 11.22215374030649926, 45.56218137147968861, 80.55433879953099563 ) ) ;
#10476 = CARTESIAN_POINT ( 'NONE',  ( -2.970231456936518910, 51.56264740916601852, 78.78030711080756987 ) ) ;
#10477 = CARTESIAN_POINT ( 'NONE',  ( 1.658154530501164237, 36.04125148601230677, 72.45433879953085921 ) ) ;
#10478 = FACE_OUTER_BOUND ( 'NONE', #1317, .T. ) ;
#10479 = CARTESIAN_POINT ( 'NONE',  ( 0.3906990944827833934, 52.35576236765771796, 78.86056079792015794 ) ) ;
#10480 = ORIENTED_EDGE ( 'NONE', *, *, #12099, .T. ) ;
#10481 = LINE ( 'NONE', #16947, #13266 ) ;
#10482 = CIRCLE ( 'NONE', #936, 8.199999999999995737 ) ;
#10483 = ORIENTED_EDGE ( 'NONE', *, *, #17243, .T. ) ;
#10484 = LINE ( 'NONE', #8982, #5369 ) ;
#10485 = LINE ( 'NONE', #7152, #10790 ) ;
#10486 = CYLINDRICAL_SURFACE ( 'NONE', #11830, 8.799999999999995381 ) ;
#10487 = DIRECTION ( 'NONE',  ( -5.626130192357176673E-16, -1.831515347669941892E-30, 1.000000000000000000 ) ) ;
#10488 = CARTESIAN_POINT ( 'NONE',  ( -1.392380047608623439, 49.84925249003585179, 53.23980501161587853 ) ) ;
#10489 = VECTOR ( 'NONE', #5768, 1000.000000000000000 ) ;
#10490 = CARTESIAN_POINT ( 'NONE',  ( 0.2541436421823697334, 38.02374091943176637, 95.29808879782397923 ) ) ;
#10491 = CARTESIAN_POINT ( 'NONE',  ( -5.679243918435851413, 37.80248940946449210, 75.65168154244369703 ) ) ;
#10492 = ORIENTED_EDGE ( 'NONE', *, *, #19223, .F. ) ;
#10493 = CARTESIAN_POINT ( 'NONE',  ( 4.133950555568060459, 51.52399475064406431, 77.16541282331252205 ) ) ;
#10494 = AXIS2_PLACEMENT_3D ( 'NONE', #19075, #4582, #1407 ) ;
#10495 = ORIENTED_EDGE ( 'NONE', *, *, #2583, .T. ) ;
#10496 = CARTESIAN_POINT ( 'NONE',  ( 23.03948732994508930, 27.61837231449496599, 76.90433879953101837 ) ) ;
#10497 = CARTESIAN_POINT ( 'NONE',  ( 4.987494971863720927, 47.58855820898865829, 94.71121379953099506 ) ) ;
#10498 = CARTESIAN_POINT ( 'NONE',  ( -3.943187491250720544, 40.73580453397070755, 91.58621379953098085 ) ) ;
#10499 = VERTEX_POINT ( 'NONE', #7396 ) ;
#10500 = CARTESIAN_POINT ( 'NONE',  ( 6.828503391016846891, 43.33193468930419101, 92.91433880123798872 ) ) ;
#10501 = CARTESIAN_POINT ( 'NONE',  ( 0.3896696312604364665, 52.96120322344530962, 77.46089148198416297 ) ) ;
#10502 = CARTESIAN_POINT ( 'NONE',  ( -4.901157372041539340, 42.48549306292126460, 95.05433879953096721 ) ) ;
#10503 = CARTESIAN_POINT ( 'NONE',  ( -4.618682869335207108, 51.30449996580257022, 78.93596273702843291 ) ) ;
#10504 = CARTESIAN_POINT ( 'NONE',  ( 5.544968037009670780, 45.50804040601273925, 92.13308879953099506 ) ) ;
#10505 = VERTEX_POINT ( 'NONE', #20581 ) ;
#10506 = CARTESIAN_POINT ( 'NONE',  ( 1.419815960288714596, 52.31341683702156331, 79.43674840306717044 ) ) ;
#10507 = ORIENTED_EDGE ( 'NONE', *, *, #8625, .F. ) ;
#10508 = PLANE ( 'NONE',  #2946 ) ;
#10509 = CARTESIAN_POINT ( 'NONE',  ( 2.263811127080450625, 49.90383875825364157, 85.41268141275705261 ) ) ;
#10510 = AXIS2_PLACEMENT_3D ( 'NONE', #9104, #15592, #16868 ) ;
#10511 = CARTESIAN_POINT ( 'NONE',  ( -4.530495696546473994, 37.70859131435868505, 76.21310604893328389 ) ) ;
#10512 = CARTESIAN_POINT ( 'NONE',  ( 0.5221537403065076299, 49.16218137147969003, 94.29136871766880290 ) ) ;
#10513 = CARTESIAN_POINT ( 'NONE',  ( -3.105924918850441863, 36.80844641393417760, 78.65049157520557799 ) ) ;
#10514 = VERTEX_POINT ( 'NONE', #13885 ) ;
#10515 = VERTEX_POINT ( 'NONE', #6007 ) ;
#10516 = ADVANCED_FACE ( 'NONE', ( #17499, #10728 ), #13997, .F. ) ;
#10517 = DIRECTION ( 'NONE',  ( 0.3165065846431827645, 0.9485903129789529098, 0.000000000000000000 ) ) ;
#10518 = ORIENTED_EDGE ( 'NONE', *, *, #17456, .T. ) ;
#10519 = FACE_OUTER_BOUND ( 'NONE', #10397, .T. ) ;
#10520 = CARTESIAN_POINT ( 'NONE',  ( -0.7268458593731683681, 40.36218137147969998, 46.35433879953098568 ) ) ;
#10521 = CARTESIAN_POINT ( 'NONE',  ( -7.203525358565210368, 41.41373112547281465, 78.69802495076405080 ) ) ;
#10522 = ORIENTED_EDGE ( 'NONE', *, *, #10042, .T. ) ;
#10523 = VECTOR ( 'NONE', #17413, 1000.000000000000227 ) ;
#10524 = ORIENTED_EDGE ( 'NONE', *, *, #17672, .T. ) ;
#10525 = FACE_OUTER_BOUND ( 'NONE', #19094, .T. ) ;
#10526 = EDGE_LOOP ( 'NONE', ( #8086, #17013, #1782, #14582 ) ) ;
#10527 = CARTESIAN_POINT ( 'NONE',  ( -4.677846259693496656, 44.16218127507082158, 94.26911326394257173 ) ) ;
#10528 = DIRECTION ( 'NONE',  ( -0.3165065846431928120, -0.9485903129789495791, -2.188653791613883869E-16 ) ) ;
#10529 = EDGE_CURVE ( 'NONE', #12799, #531, #9423, .T. ) ;
#10530 = CARTESIAN_POINT ( 'NONE',  ( 3.460444912181559474, 49.25145096859824889, 92.99246380123805977 ) ) ;
#10531 = CARTESIAN_POINT ( 'NONE',  ( 4.125939684684055919, 51.51579152172704568, 77.12434737327507150 ) ) ;
#10532 = DIRECTION ( 'NONE',  ( 1.110223024625156540E-16, 1.000000000000000000, 5.922860397471808077E-17 ) ) ;
#10533 = LINE ( 'NONE', #832, #1152 ) ;
#10534 = CARTESIAN_POINT ( 'NONE',  ( 8.787842894572216679, 41.13144714757795128, 76.38644048143638088 ) ) ;
#10535 = CARTESIAN_POINT ( 'NONE',  ( 29.03948732994507864, 36.35905713404685002, 74.70433879953100131 ) ) ;
#10536 = CARTESIAN_POINT ( 'NONE',  ( -4.677846234370045764, 43.47758828951683796, 94.29575777171292827 ) ) ;
#10537 = CARTESIAN_POINT ( 'NONE',  ( 5.544968037009670780, 45.50804040601273925, 92.44558880294498238 ) ) ;
#10538 = ADVANCED_FACE ( 'NONE', ( #17290 ), #10927, .F. ) ;
#10539 = CARTESIAN_POINT ( 'NONE',  ( -7.368313902600233334, 41.94587499716005397, 78.71972396713441356 ) ) ;
#10540 = VERTEX_POINT ( 'NONE', #14303 ) ;
#10541 = CARTESIAN_POINT ( 'NONE',  ( 8.924621998940734713, 41.54138280047497744, 78.88894238123772595 ) ) ;
#10542 = ADVANCED_FACE ( 'NONE', ( #19400 ), #10741, .T. ) ;
#10543 = ADVANCED_FACE ( 'NONE', ( #11339, #14619 ), #3334, .T. ) ;
#10544 = MECHANICAL_DESIGN_GEOMETRIC_PRESENTATION_REPRESENTATION (  '', ( #15668 ), #12889 ) ;
#10545 = ORIENTED_EDGE ( 'NONE', *, *, #5873, .T. ) ;
#10546 = CARTESIAN_POINT ( 'NONE',  ( -1.477846259693502917, 47.62628298661744708, 77.15433879953100416 ) ) ;
#10547 = VECTOR ( 'NONE', #19194, 1000.000000000000000 ) ;
#10548 = CARTESIAN_POINT ( 'NONE',  ( 11.22215374030650281, 48.36218137147968577, 54.55433879953099563 ) ) ;
#10549 = CARTESIAN_POINT ( 'NONE',  ( -3.387980870927748800, 52.18391455498849751, 78.68920376838389075 ) ) ;
#10550 = CARTESIAN_POINT ( 'NONE',  ( 5.568489401881125289, 48.03437091500646261, 93.07058880123797451 ) ) ;
#10551 = DIRECTION ( 'NONE',  ( 1.540237394707284220E-16, 1.793354297423764243E-16, -1.000000000000000000 ) ) ;
#10552 = CARTESIAN_POINT ( 'NONE',  ( -6.989009964201624570, 47.26660036502315876, 78.95058778273427436 ) ) ;
#10553 = CARTESIAN_POINT ( 'NONE',  ( 8.648170029844118645, 43.06315486489794608, 77.06316232894263862 ) ) ;
#10554 = EDGE_CURVE ( 'NONE', #8776, #18462, #5495, .T. ) ;
#10555 = DIRECTION ( 'NONE',  ( -0.9485903129789527988, 0.3165065846431829311, -8.934458285744989980E-17 ) ) ;
#10556 = VECTOR ( 'NONE', #5420, 1000.000000000000114 ) ;
#10557 = VERTEX_POINT ( 'NONE', #348 ) ;
#10558 = ORIENTED_EDGE ( 'NONE', *, *, #30, .F. ) ;
#10559 = CARTESIAN_POINT ( 'NONE',  ( 8.584650940598146818, 42.88688602177342091, 79.09515810002898206 ) ) ;
#10560 = DIRECTION ( 'NONE',  ( 1.540237394707284220E-16, 1.793354297423764243E-16, -1.000000000000000000 ) ) ;
#10561 = DIRECTION ( 'NONE',  ( -0.000000000000000000, 1.000000000000000000, 1.734723475976787531E-14 ) ) ;
#10562 = CARTESIAN_POINT ( 'NONE',  ( 5.934652055452926511, 51.10460149980519873, 77.05868164888072158 ) ) ;
#10563 = B_SPLINE_SURFACE_WITH_KNOTS ( 'NONE', 3, 1, ( 
 ( #9057, #14046 ),
 ( #9164, #9376 ),
 ( #12764, #15544 ),
 ( #7562, #12668 ),
 ( #19149, #20836 ),
 ( #15859, #14246 ),
 ( #20529, #6056 ),
 ( #1273, #4560 ),
 ( #962, #6364 ),
 ( #16485, #3390 ),
 ( #9695, #11604 ) ),
 .UNSPECIFIED., .F., .F., .F.,
 ( 4, 1, 1, 1, 1, 1, 1, 1, 4 ),
 ( 2, 2 ),
 ( 0.000000000000000000, 0.1077815449370134182, 0.2006545494464173907, 0.2847368448845932765, 0.3681045469499393263, 0.4695596479522798350, 0.6076740370479670750, 0.7836404280850621795, 1.000000000000000000 ),
 ( 0.000000000000000000, 1.000000000000000000 ),
 .UNSPECIFIED. ) ;
#10564 = CARTESIAN_POINT ( 'NONE',  ( -1.477846259693486486, 49.81903562097206617, 123.5543387995310098 ) ) ;
#10565 = VECTOR ( 'NONE', #19913, 1000.000000000000000 ) ;
#10566 = DIRECTION ( 'NONE',  ( -5.626130192357176673E-16, -1.831515347669941892E-30, 1.000000000000000000 ) ) ;
#10567 = CARTESIAN_POINT ( 'NONE',  ( 5.025485839985549319, 41.56218137147963887, 91.03933880294498238 ) ) ;
#10568 = CARTESIAN_POINT ( 'NONE',  ( 2.263811127080455954, 49.90383875825364157, 53.41268141275705972 ) ) ;
#10569 = CARTESIAN_POINT ( 'NONE',  ( -5.889261015154382051, 37.95762057880577345, 79.03330530165142420 ) ) ;
#10570 = VECTOR ( 'NONE', #10107, 1000.000000000000000 ) ;
#10571 = EDGE_CURVE ( 'NONE', #18616, #10028, #3966, .T. ) ;
#10572 = CARTESIAN_POINT ( 'NONE',  ( 6.721999984869559519, 37.77659228945417880, 75.79056106475293575 ) ) ;
#10573 = ORIENTED_EDGE ( 'NONE', *, *, #3883, .F. ) ;
#10574 = ADVANCED_FACE ( 'NONE', ( #7043 ), #6938, .T. ) ;
#10575 = FACE_OUTER_BOUND ( 'NONE', #430, .T. ) ;
#10576 = EDGE_LOOP ( 'NONE', ( #4965, #11035, #10670, #9786, #3796, #8484, #3786, #4597 ) ) ;
#10577 = VECTOR ( 'NONE', #17873, 1000.000000000000000 ) ;
#10578 = CARTESIAN_POINT ( 'NONE',  ( -4.446085291674333639, 50.68091644337815893, 78.65631888207801126 ) ) ;
#10579 = EDGE_CURVE ( 'NONE', #2608, #16492, #11835, .T. ) ;
#10580 = CARTESIAN_POINT ( 'NONE',  ( -3.981178359372548492, 46.76218137147973408, 95.41433880294498238 ) ) ;
#10581 = ORIENTED_EDGE ( 'NONE', *, *, #4303, .T. ) ;
#10582 = CARTESIAN_POINT ( 'NONE',  ( -4.007890887056452023, 40.01116025973682611, 94.04808879782399345 ) ) ;
#10583 = EDGE_CURVE ( 'NONE', #19292, #10724, #15188, .T. ) ;
#10584 = ADVANCED_FACE ( 'NONE', ( #8554 ), #18329, .F. ) ;
#10585 = CARTESIAN_POINT ( 'NONE',  ( 11.22215374030649926, 51.36218137147968577, 70.80574467885102763 ) ) ;
#10586 = DIRECTION ( 'NONE',  ( -0.3219511000281078394, 0.002538702742701116205, -0.9467528949937651372 ) ) ;
#10587 = DIRECTION ( 'NONE',  ( 5.626130192357176673E-16, 1.831515347669941892E-30, -1.000000000000000000 ) ) ;
#10588 = CARTESIAN_POINT ( 'NONE',  ( 0.4974180460467604870, 52.36224188547572567, 77.38972066725763455 ) ) ;
#10589 = CARTESIAN_POINT ( 'NONE',  ( -4.189188114579794231, 36.70184521026505564, 79.48068319027247242 ) ) ;
#10590 = EDGE_LOOP ( 'NONE', ( #17075, #2417, #18693, #318 ) ) ;
#10591 = AXIS2_PLACEMENT_3D ( 'NONE', #17064, #20341, #5780 ) ;
#10592 = CARTESIAN_POINT ( 'NONE',  ( 8.245414686166476770, 41.40667145630854407, 77.48117334564075520 ) ) ;
#10593 = VERTEX_POINT ( 'NONE', #2168 ) ;
#10594 = LINE ( 'NONE', #7262, #285 ) ;
#10595 = CARTESIAN_POINT ( 'NONE',  ( 4.629792079547915939, 52.06844900104020013, 77.37197156638603701 ) ) ;
#10596 = CARTESIAN_POINT ( 'NONE',  ( 6.912263059922415742, 50.38247963137696672, 77.24227907682649175 ) ) ;
#10597 = LINE ( 'NONE', #4274, #681 ) ;
#10598 = CARTESIAN_POINT ( 'NONE',  ( 6.266852414816192152, 50.85921847619028568, 79.48482414599367019 ) ) ;
#10599 = LINE ( 'NONE', #5665, #13533 ) ;
#10600 = CARTESIAN_POINT ( 'NONE',  ( 4.673174852049361228, 39.63213674411673537, 94.20433879782400766 ) ) ;
#10601 = CARTESIAN_POINT ( 'NONE',  ( -4.948764291328625831, 37.26291353443464516, 75.36972643424059015 ) ) ;
#10602 = ORIENTED_EDGE ( 'NONE', *, *, #14917, .F. ) ;
#10603 = CARTESIAN_POINT ( 'NONE',  ( 8.837344731589771740, 41.27980729345753730, 78.92656146296575059 ) ) ;
#10604 = VECTOR ( 'NONE', #11524, 1000.000000000000114 ) ;
#10605 = ORIENTED_EDGE ( 'NONE', *, *, #354, .T. ) ;
#10606 = CARTESIAN_POINT ( 'NONE',  ( -4.383473025373059606, 51.47257230871590394, 78.45066232894264147 ) ) ;
#10607 = EDGE_CURVE ( 'NONE', #2282, #5117, #15148, .T. ) ;
#10608 = CARTESIAN_POINT ( 'NONE',  ( 6.102441102155617969, 43.42752260303680600, 94.55496379953098085 ) ) ;
#10609 = PRODUCT ( 'Shackle', 'Shackle', '', ( #2407 ) ) ;
#10610 = ORIENTED_EDGE ( 'NONE', *, *, #18862, .F. ) ;
#10611 = CARTESIAN_POINT ( 'NONE',  ( 1.352400422481993658, 50.46853102219002096, 94.47683880123798872 ) ) ;
#10612 = CARTESIAN_POINT ( 'NONE',  ( 2.463659247115866258, 38.82793883177424732, 94.12621379782399345 ) ) ;
#10613 = CARTESIAN_POINT ( 'NONE',  ( 0.5221537403065013017, 44.16218137147968292, 76.96022115247204454 ) ) ;
#10614 = VERTEX_POINT ( 'NONE', #10380 ) ;
#10615 = DIRECTION ( 'NONE',  ( 2.409338161078896715E-16, -1.000000000000000000, 0.000000000000000000 ) ) ;
#10616 = CARTESIAN_POINT ( 'NONE',  ( 27.03948732994508930, 36.35905713404685713, 78.30433879953100984 ) ) ;
#10617 = ORIENTED_EDGE ( 'NONE', *, *, #12741, .T. ) ;
#10618 = CARTESIAN_POINT ( 'NONE',  ( 1.652727357819364418, 35.35299279957455099, 76.16022115247204738 ) ) ;
#10619 = CIRCLE ( 'NONE', #9933, 8.199999999999995737 ) ;
#10620 = ORIENTED_EDGE ( 'NONE', *, *, #9540, .F. ) ;
#10621 = CARTESIAN_POINT ( 'NONE',  ( -3.988948728167713398, 41.15132427329136533, 92.45433879953091605 ) ) ;
#10622 = PLANE ( 'NONE',  #5778 ) ;
#10623 = AXIS2_PLACEMENT_3D ( 'NONE', #1688, #6458, #18064 ) ;
#10624 = DIRECTION ( 'NONE',  ( 0.000000000000000000, 0.000000000000000000, 1.000000000000000000 ) ) ;
#10625 = APPLICATION_PROTOCOL_DEFINITION ( 'draft international standard', 'automotive_design', 1998, #7770 ) ;
#10626 = CARTESIAN_POINT ( 'NONE',  ( -4.448275204524981596, 37.64785834894585292, 75.98775578934684916 ) ) ;
#10627 = CARTESIAN_POINT ( 'NONE',  ( 5.254713546219920595, 50.85372921038054983, 78.82175487302160377 ) ) ;
#10628 = DIRECTION ( 'NONE',  ( -0.000000000000000000, 1.000000000000000000, -0.000000000000000000 ) ) ;
#10629 = EDGE_CURVE ( 'NONE', #5410, #3669, #13542, .T. ) ;
#10630 = VERTEX_POINT ( 'NONE', #5450 ) ;
#10631 = LINE ( 'NONE', #17100, #15968 ) ;
#10632 = ORIENTED_EDGE ( 'NONE', *, *, #9923, .F. ) ;
#10633 = AXIS2_PLACEMENT_3D ( 'NONE', #6499, #4586, #6192 ) ;
#10634 = CARTESIAN_POINT ( 'NONE',  ( 2.122153740306512937, 50.16218137147969713, 53.55433879953100273 ) ) ;
#10635 = CARTESIAN_POINT ( 'NONE',  ( 10.77494014480653561, 42.96218137147968008, 73.80433879953100984 ) ) ;
#10636 = CARTESIAN_POINT ( 'NONE',  ( 3.788215052820487205, 39.19523464621513398, 90.24306233796824017 ) ) ;
#10637 = VECTOR ( 'NONE', #17365, 1000.000000000000114 ) ;
#10638 = ORIENTED_EDGE ( 'NONE', *, *, #16944, .F. ) ;
#10639 = CARTESIAN_POINT ( 'NONE',  ( 6.632598449108662031, 50.58905661380737939, 79.28554042632779897 ) ) ;
#10640 = ORIENTED_EDGE ( 'NONE', *, *, #18075, .T. ) ;
#10641 = CARTESIAN_POINT ( 'NONE',  ( 2.522153740306511960, 47.62628298661745418, 45.55433879953100273 ) ) ;
#10642 = DIRECTION ( 'NONE',  ( 0.8043570849667761591, -0.5941461771851692664, 1.733862608106489734E-17 ) ) ;
#10643 = CARTESIAN_POINT ( 'NONE',  ( 7.672912595070442876, 40.17111506963394163, 76.58175473889373563 ) ) ;
#10644 = CARTESIAN_POINT ( 'NONE',  ( -1.477846259693490705, 49.81903562097208038, 61.15433879953099705 ) ) ;
#10645 = CARTESIAN_POINT ( 'NONE',  ( 4.567922609689349045, 52.11414948617044729, 77.12434737327507150 ) ) ;
#10646 = CARTESIAN_POINT ( 'NONE',  ( -7.609226043662618899, 43.10354341710602455, 78.64709103647231814 ) ) ;
#10647 = DIRECTION ( 'NONE',  ( -0.5941461771851691553, -0.8043570849667760481, -2.357623395011396791E-16 ) ) ;
#10648 = CARTESIAN_POINT ( 'NONE',  ( 4.470572738639666532, 36.16780480931087283, 79.45433879953087342 ) ) ;
#10649 = EDGE_CURVE ( 'NONE', #7228, #14869, #18441, .T. ) ;
#10651 = CARTESIAN_POINT ( 'NONE',  ( -5.383807009170671343, 49.83799468618045836, 76.28720437108826502 ) ) ;
#10650 = CIRCLE ( 'NONE', #20458, 4.999999999999997335 ) ;
#10652 = CARTESIAN_POINT ( 'NONE',  ( 6.102441102155617969, 43.42752260303680600, 91.11746380294498238 ) ) ;
#10653 = VECTOR ( 'NONE', #2318, 999.9999999999998863 ) ;
#10654 = DIRECTION ( 'NONE',  ( -1.111814006898795283E-16, 5.922860397471810542E-17, -1.000000000000000000 ) ) ;
#10655 = CARTESIAN_POINT ( 'NONE',  ( 8.306444873683641816, 41.60874232747575263, 78.93548851266230315 ) ) ;
#10656 = EDGE_CURVE ( 'NONE', #15803, #14953, #20128, .T. ) ;
#10657 = ORIENTED_EDGE ( 'NONE', *, *, #18870, .F. ) ;
#10658 = B_SPLINE_CURVE_WITH_KNOTS ( 'NONE', 3,
 ( #17899, #9826, #6717, #8729, #11530, #3427 ),
 .UNSPECIFIED., .F., .F.,
 ( 4, 2, 4 ),
 ( 0.000000000000000000, 0.001381175314065558610, 0.002762350628131117220 ),
 .UNSPECIFIED. ) ;
#10659 = DIRECTION ( 'NONE',  ( -1.402518428993831676E-16, 1.000000000000000000, -0.000000000000000000 ) ) ;
#10660 = EDGE_CURVE ( 'NONE', #12054, #11891, #10485, .T. ) ;
#10661 = LINE ( 'NONE', #17124, #3117 ) ;
#10662 = LINE ( 'NONE', #12034, #9285 ) ;
#10663 = CARTESIAN_POINT ( 'NONE',  ( -7.677846259693485109, 51.36218137147968577, 93.55433879953098142 ) ) ;
#10664 = VECTOR ( 'NONE', #15033, 1000.000000000000114 ) ;
#10665 = CARTESIAN_POINT ( 'NONE',  ( 6.880132251722071324, 48.33664052787082710, 75.45433879953087342 ) ) ;
#10666 = CARTESIAN_POINT ( 'NONE',  ( 0.3326973149608335456, 52.96014171822455552, 77.76169174070734869 ) ) ;
#10667 = CARTESIAN_POINT ( 'NONE',  ( 5.467161035934759994, 36.87993031913157438, 77.68578589458712713 ) ) ;
#10668 = CARTESIAN_POINT ( 'NONE',  ( 0.5221537403065064087, 48.16218137147969003, 77.55433879953099563 ) ) ;
#10669 = ORIENTED_EDGE ( 'NONE', *, *, #9675, .T. ) ;
#10670 = ORIENTED_EDGE ( 'NONE', *, *, #2780, .T. ) ;
#10671 = CARTESIAN_POINT ( 'NONE',  ( 9.060635047751631532, 41.94902253626816702, 79.49775514261133935 ) ) ;
#10672 = CARTESIAN_POINT ( 'NONE',  ( -4.151536175905484072, 36.67403323987894481, 75.43521673441158271 ) ) ;
#10673 = CARTESIAN_POINT ( 'NONE',  ( 8.868817592801743643, 41.37413345511091478, 75.97198585835440099 ) ) ;
#10674 = DIRECTION ( 'NONE',  ( 1.000000000000000000, -1.110223024625156540E-16, 1.779391786395883043E-16 ) ) ;
#10675 = LINE ( 'NONE', #18301, #19616 ) ;
#10676 = CARTESIAN_POINT ( 'NONE',  ( -4.249412910294118717, 50.83092575845958550, 78.93669174070734584 ) ) ;
#10677 = CARTESIAN_POINT ( 'NONE',  ( 5.544968037009670780, 45.50804040601273925, 89.94558880294498238 ) ) ;
#10678 = CARTESIAN_POINT ( 'NONE',  ( -4.283496025856504019, 47.84326572019833179, 75.45433879953087342 ) ) ;
#10679 = VECTOR ( 'NONE', #7233, 1000.000000000000000 ) ;
#10680 = DIRECTION ( 'NONE',  ( 1.540237394707284220E-16, 1.793354297423764243E-16, -1.000000000000000000 ) ) ;
#10681 = CARTESIAN_POINT ( 'NONE',  ( 0.5221537403065014127, 44.16218137147968292, 76.16022115247204738 ) ) ;
#10682 = EDGE_CURVE ( 'NONE', #10795, #8152, #5565, .T. ) ;
#10683 = CARTESIAN_POINT ( 'NONE',  ( 6.136807603568960268, 37.35843523903731977, 75.40772603260481333 ) ) ;
#10684 = ORIENTED_EDGE ( 'NONE', *, *, #8192, .T. ) ;
#10685 = CARTESIAN_POINT ( 'NONE',  ( 5.394726803408533833, 50.74878659197170094, 77.28963291717792572 ) ) ;
#10686 = ORIENTED_EDGE ( 'NONE', *, *, #2970, .T. ) ;
#10687 = FACE_OUTER_BOUND ( 'NONE', #8915, .T. ) ;
#10688 = CARTESIAN_POINT ( 'NONE',  ( 5.025485839985549319, 41.56218137147963887, 94.78933880294496817 ) ) ;
#10689 =( BOUNDED_CURVE ( )  B_SPLINE_CURVE ( 3, ( #1599, #5089, #12600, #17865 ),
 .UNSPECIFIED., .F., .F. ) 
 B_SPLINE_CURVE_WITH_KNOTS ( ( 4, 4 ),
 ( 4.565792013076894307, 4.566698375078894756 ),
 .UNSPECIFIED. ) 
 CURVE ( )  GEOMETRIC_REPRESENTATION_ITEM ( )  RATIONAL_B_SPLINE_CURVE ( ( 1.000000000000000000, 0.9999999315423278023, 0.9999999315423278023, 1.000000000000000000 ) ) 
 REPRESENTATION_ITEM ( '' )  );
#10690 = VERTEX_POINT ( 'NONE', #18548 ) ;
#10691 = CARTESIAN_POINT ( 'NONE',  ( 31.07218010054375412, 42.76218137147968434, 70.80574467885102763 ) ) ;
#10692 = VECTOR ( 'NONE', #20052, 1000.000000000000114 ) ;
#10693 = CARTESIAN_POINT ( 'NONE',  ( -0.5881641420295652400, 52.97589590771117685, 75.69129100417544009 ) ) ;
#10694 = CARTESIAN_POINT ( 'NONE',  ( -2.990358918575095171, 51.54826506199249536, 78.86270620133520026 ) ) ;
#10695 = CARTESIAN_POINT ( 'NONE',  ( -1.477846259693498920, 49.81903562097206617, 75.21119304902337888 ) ) ;
#10696 = CARTESIAN_POINT ( 'NONE',  ( 5.273270741223392122, 50.83850129255925054, 77.24912405724838038 ) ) ;
#10697 = CARTESIAN_POINT ( 'NONE',  ( -3.096855864432994210, 36.80899838413677827, 78.50831005042292077 ) ) ;
#10698 = ORIENTED_EDGE ( 'NONE', *, *, #253, .T. ) ;
#10699 = EDGE_CURVE ( 'NONE', #10155, #7140, #3961, .T. ) ;
#10700 = CARTESIAN_POINT ( 'NONE',  ( 8.214799251806553571, 41.32260305165857517, 77.14698585835439815 ) ) ;
#10701 = ORIENTED_EDGE ( 'NONE', *, *, #12761, .F. ) ;
#10702 = CARTESIAN_POINT ( 'NONE',  ( 5.658108625003792191, 37.01637447524286273, 75.97198585835440099 ) ) ;
#10703 = EDGE_CURVE ( 'NONE', #6648, #7726, #241, .T. ) ;
#10704 = FACE_OUTER_BOUND ( 'NONE', #10526, .T. ) ;
#10705 = CARTESIAN_POINT ( 'NONE',  ( -1.579458713458412822, 38.67424504376464967, 92.55433879953098142 ) ) ;
#10706 = CARTESIAN_POINT ( 'NONE',  ( 6.632598449108662031, 50.58905661380737939, 79.28554042632779897 ) ) ;
#10707 = DIRECTION ( 'NONE',  ( -0.4999999999999984457, -0.8660254037844394848, -0.000000000000000000 ) ) ;
#10708 = LINE ( 'NONE', #18967, #464 ) ;
#10709 = CARTESIAN_POINT ( 'NONE',  ( 6.217311209797515836, 50.06224385580732417, 79.30230994520773891 ) ) ;
#10710 = EDGE_CURVE ( 'NONE', #8000, #10285, #19713, .T. ) ;
#10711 = ADVANCED_FACE ( 'NONE', ( #20454 ), #17650, .F. ) ;
#10712 = ORIENTED_EDGE ( 'NONE', *, *, #14551, .T. ) ;
#10713 = CARTESIAN_POINT ( 'NONE',  ( 4.437233947525204059, 51.36737272290800860, 77.60409055468527129 ) ) ;
#10714 = EDGE_CURVE ( 'NONE', #17824, #5907, #13863, .T. ) ;
#10715 = ORIENTED_EDGE ( 'NONE', *, *, #2952, .F. ) ;
#10716 = FACE_OUTER_BOUND ( 'NONE', #13681, .T. ) ;
#10717 = CARTESIAN_POINT ( 'NONE',  ( -3.981178359372548492, 46.76218137147973408, 96.35183879953099506 ) ) ;
#10718 = CARTESIAN_POINT ( 'NONE',  ( -7.302678038849692577, 42.15150420378952845, 77.34580771017452605 ) ) ;
#10719 = ORIENTED_EDGE ( 'NONE', *, *, #6772, .T. ) ;
#10720 = CARTESIAN_POINT ( 'NONE',  ( 1.352400422481993658, 50.46853102219002096, 91.97683880123797451 ) ) ;
#10721 = FACE_BOUND ( 'NONE', #8141, .T. ) ;
#10722 = CARTESIAN_POINT ( 'NONE',  ( -0.2947060777460364656, 38.91366773902584697, 95.05433879953096721 ) ) ;
#10723 = CARTESIAN_POINT ( 'NONE',  ( -4.705661087595403025, 51.24234851550965431, 78.91934866582661812 ) ) ;
#10724 = VERTEX_POINT ( 'NONE', #4067 ) ;
#10725 = LINE ( 'NONE', #4296, #2719 ) ;
#10726 = CARTESIAN_POINT ( 'NONE',  ( 0.7513193414822582072, 52.35291871808690445, 78.87878230117789258 ) ) ;
#10727 = ORIENTED_EDGE ( 'NONE', *, *, #3536, .T. ) ;
#10728 = FACE_BOUND ( 'NONE', #9699, .T. ) ;
#10729 = CARTESIAN_POINT ( 'NONE',  ( 2.927603783594689979, 51.37146775011972011, 72.45433879953087342 ) ) ;
#10730 = APPLICATION_PROTOCOL_DEFINITION ( 'draft international standard', 'automotive_design', 1998, #2327 ) ;
#10731 = CARTESIAN_POINT ( 'NONE',  ( 5.581823371501742237, 36.96186382607169207, 75.98067903659783440 ) ) ;
#10732 = EDGE_CURVE ( 'NONE', #8473, #5980, #1102, .T. ) ;
#10733 = CARTESIAN_POINT ( 'NONE',  ( 5.455409717288331350, 36.87153325707006957, 76.14053225265315916 ) ) ;
#10734 = DIRECTION ( 'NONE',  ( 0.3164953060534052010, 0.9485565103298893019, -0.008442035118619106368 ) ) ;
#10735 = EDGE_LOOP ( 'NONE', ( #19799, #4521, #16780, #19857 ) ) ;
#10736 = CARTESIAN_POINT ( 'NONE',  ( 1.702985681980708321, 52.20476652859439071, 75.60954117182248524 ) ) ;
#10737 = VERTEX_POINT ( 'NONE', #15682 ) ;
#10738 = DIRECTION ( 'NONE',  ( -0.3165065846431826535, -0.9485903129789529098, -2.188653791613874008E-16 ) ) ;
#10739 = CARTESIAN_POINT ( 'NONE',  ( 0.3869604771732107484, 52.35579184508003436, 77.46088296688223807 ) ) ;
#10740 = CARTESIAN_POINT ( 'NONE',  ( -4.567115856812060670, 47.10047254335474065, 94.55496380123798872 ) ) ;
#10741 = B_SPLINE_SURFACE_WITH_KNOTS ( 'NONE', 3, 1, ( 
 ( #6624, #6214 ),
 ( #144, #6412 ),
 ( #17810, #17597 ),
 ( #4817, #9639 ),
 ( #11543, #13128 ),
 ( #1757, #19603 ),
 ( #20780, #6523 ),
 ( #8237, #5025 ),
 ( #8024, #12714 ),
 ( #17705, #14724 ),
 ( #18020, #12921 ),
 ( #3135, #3441 ),
 ( #11127, #17911 ),
 ( #11234, #1857 ),
 ( #12810, #19293 ),
 ( #9954, #19192 ),
 ( #45, #4706 ),
 ( #16219, #4607 ),
 ( #20879, #16438 ) ),
 .UNSPECIFIED., .F., .F., .F.,
 ( 4, 1, 1, 1, 1, 1, 1, 1, 1, 1, 1, 1, 1, 1, 1, 1, 4 ),
 ( 2, 2 ),
 ( 0.000000000000000000, 0.07819787255609964016, 0.1515336364311310191, 0.2187066978088008651, 0.2814522326392254747, 0.3385163222030129759, 0.3915958516965070690, 0.4406923075239814191, 0.4864642379862412769, 0.5323932679607442653, 0.5831133966729620255, 0.6391356099194271945, 0.6992555458516984679, 0.7657124642625251498, 0.8379597225178306852, 0.9162365097749198828, 1.000000000000000000 ),
 ( 0.000000000000000000, 1.000000000000000000 ),
 .UNSPECIFIED. ) ;
#10742 = ORIENTED_EDGE ( 'NONE', *, *, #12095, .T. ) ;
#10743 = CARTESIAN_POINT ( 'NONE',  ( -4.303670962001103106, 50.79176777958974753, 75.36022115247205022 ) ) ;
#10744 = ORIENTED_EDGE ( 'NONE', *, *, #15451, .T. ) ;
#10745 = FACE_OUTER_BOUND ( 'NONE', #12425, .T. ) ;
#10746 = CARTESIAN_POINT ( 'NONE',  ( -3.566438244846301231, 38.23101125920473464, 76.53375056423675460 ) ) ;
#10747 = CARTESIAN_POINT ( 'NONE',  ( 8.401796425420881675, 39.97444138920005230, 76.12035193564865665 ) ) ;
#10748 = CARTESIAN_POINT ( 'NONE',  ( -0.4699484075729998267, 52.36218137147968577, 87.21440135111343750 ) ) ;
#10749 = CARTESIAN_POINT ( 'NONE',  ( -7.645086356741528810, 40.78432135352825583, 79.43600262374511090 ) ) ;
#10750 = CARTESIAN_POINT ( 'NONE',  ( -7.611066721457015127, 43.11777894428342961, 78.46404369028466874 ) ) ;
#10751 = CARTESIAN_POINT ( 'NONE',  ( -5.004817973257478236, 39.29348442311233214, 78.18375056423674607 ) ) ;
#10752 = CARTESIAN_POINT ( 'NONE',  ( -2.313335635445065375, 37.76218137147968434, 96.05433879953096721 ) ) ;
#10753 = DIRECTION ( 'NONE',  ( -0.9485903129789527988, 0.3165065846431829311, -8.934458285744989980E-17 ) ) ;
#10754 = CARTESIAN_POINT ( 'NONE',  ( -0.2125050281363792815, 38.58189400963056670, 94.55496380294496817 ) ) ;
#10755 = CARTESIAN_POINT ( 'NONE',  ( 5.025485839985549319, 41.56218137147963887, 94.78933880294496817 ) ) ;
#10756 = CARTESIAN_POINT ( 'NONE',  ( -1.219503646467429814, 49.90383875825364157, 53.41268141275706682 ) ) ;
#10757 = FILL_AREA_STYLE ('',( #18821 ) ) ;
#10758 = PLANE ( 'NONE',  #8145 ) ;
#10759 = CARTESIAN_POINT ( 'NONE',  ( 31.03948732994507864, 43.16218137147969003, 78.30433879953099563 ) ) ;
#10760 = CARTESIAN_POINT ( 'NONE',  ( -3.355600405723123902, 52.20705244989922988, 78.36353918055804968 ) ) ;
#10761 = CARTESIAN_POINT ( 'NONE',  ( 6.828503391016846891, 43.33193468930419101, 90.41433880123798872 ) ) ;
#10762 = EDGE_CURVE ( 'NONE', #18313, #13475, #4178, .T. ) ;
#10763 = CARTESIAN_POINT ( 'NONE',  ( 5.748274343403733333, 51.24227120794373747, 77.94845644658968808 ) ) ;
#10764 = CARTESIAN_POINT ( 'NONE',  ( -7.203937208853350427, 41.84628966447687759, 79.54737348031042643 ) ) ;
#10765 = CARTESIAN_POINT ( 'NONE',  ( 2.484494565094232499, 50.04344131194918788, 82.45433879953087342 ) ) ;
#10766 = ORIENTED_EDGE ( 'NONE', *, *, #4563, .F. ) ;
#10767 = LINE ( 'NONE', #7444, #8032 ) ;
#10768 = CARTESIAN_POINT ( 'NONE',  ( -3.664877280008365101, 47.31003091142736849, 92.57889353644220876 ) ) ;
#10769 = CARTESIAN_POINT ( 'NONE',  ( 8.936058775400656629, 41.57565954506093675, 76.08336210994360727 ) ) ;
#10770 = CARTESIAN_POINT ( 'NONE',  ( 5.939900590116411472, 51.10072461867315496, 76.90580938776616904 ) ) ;
#10771 = CARTESIAN_POINT ( 'NONE',  ( 23.03948732994508930, 27.61837231449496599, 78.60433879953100700 ) ) ;
#10772 = DIRECTION ( 'NONE',  ( -1.000000000000000000, 1.110223024625156540E-16, 6.575695984913707633E-33 ) ) ;
#10773 = CARTESIAN_POINT ( 'NONE',  ( 13.13948732994506230, 27.61837231449496244, 78.60433879953100700 ) ) ;
#10774 = B_SPLINE_CURVE_WITH_KNOTS ( 'NONE', 3,
 ( #11541, #1537, #14407, #6307, #18018, #3233, #14617, #6520, #15123, #532, #19291, #7013 ),
 .UNSPECIFIED., .F., .F.,
 ( 4, 2, 2, 2, 2, 4 ),
 ( 0.000000000000000000, 0.0002162886299158511697, 0.0004325772598317023394, 0.0006488658897475535091, 0.0007570102047054918333, 0.0008651545196634303743 ),
 .UNSPECIFIED. ) ;
#10775 = CARTESIAN_POINT ( 'NONE',  ( -0.9387578428071298164, 52.84007946907634334, 78.24704469840057186 ) ) ;
#10776 = AXIS2_PLACEMENT_3D ( 'NONE', #14042, #4240, #11076 ) ;
#10777 = CARTESIAN_POINT ( 'NONE',  ( -7.085676915393174902, 47.03388510223538077, 78.01104965316210382 ) ) ;
#10778 = CARTESIAN_POINT ( 'NONE',  ( -5.472271698804210160, 38.58561386426530504, 78.92638042842689572 ) ) ;
#10779 = DIRECTION ( 'NONE',  ( 0.9539696396349547358, -0.2999031954727301441, 9.315070279690498823E-17 ) ) ;
#10780 = VERTEX_POINT ( 'NONE', #6366 ) ;
#10781 = EDGE_CURVE ( 'NONE', #19846, #9686, #17764, .T. ) ;
#10782 = CARTESIAN_POINT ( 'NONE',  ( 5.389492195292208798, 36.82443100924615464, 78.79551527011911105 ) ) ;
#10783 = ORIENTED_EDGE ( 'NONE', *, *, #18070, .F. ) ;
#10784 = EDGE_CURVE ( 'NONE', #4848, #16560, #4376, .T. ) ;
#10785 = CARTESIAN_POINT ( 'NONE',  ( 2.122153740306508496, 47.82824192744436687, 77.55433879953099563 ) ) ;
#10786 = CARTESIAN_POINT ( 'NONE',  ( 6.102441102155617969, 43.42752260303680600, 91.11746380294498238 ) ) ;
#10787 = VERTEX_POINT ( 'NONE', #17266 ) ;
#10788 = CARTESIAN_POINT ( 'NONE',  ( 0.2541436421823710656, 38.02374091943176637, 92.95433879782399345 ) ) ;
#10789 = CARTESIAN_POINT ( 'NONE',  ( -0.9369684686848965827, 52.97864635801455790, 77.04772206183797323 ) ) ;
#10790 = VECTOR ( 'NONE', #5131, 1000.000000000000000 ) ;
#10791 = DIRECTION ( 'NONE',  ( -0.000000000000000000, -0.000000000000000000, 1.000000000000000000 ) ) ;
#10792 = CYLINDRICAL_SURFACE ( 'NONE', #6672, 4.999999999999997335 ) ;
#10793 = CARTESIAN_POINT ( 'NONE',  ( 0.8448630204163343205, 52.35216834387308182, 76.36683753262285279 ) ) ;
#10794 = CARTESIAN_POINT ( 'NONE',  ( 3.212180877488374886, 51.27651577472676081, 75.45433879953087342 ) ) ;
#10795 = VERTEX_POINT ( 'NONE', #7263 ) ;
#10796 = ADVANCED_FACE ( 'NONE', ( #12866 ), #8879, .F. ) ;
#10797 = ORIENTED_EDGE ( 'NONE', *, *, #12820, .T. ) ;
#10798 = DIRECTION ( 'NONE',  ( -0.000000000000000000, -0.000000000000000000, 1.000000000000000000 ) ) ;
#10799 = LINE ( 'NONE', #4485, #3326 ) ;
#10800 = CARTESIAN_POINT ( 'NONE',  ( -6.792737292293178797, 47.86790251333490431, 78.78375056423675460 ) ) ;
#10801 = DIRECTION ( 'NONE',  ( -0.9534635866061451637, -0.3015081906286224411, -2.009271279954815058E-16 ) ) ;
#10802 = CARTESIAN_POINT ( 'NONE',  ( 2.921181103050038086, 49.30691215337508737, 94.75121379782399345 ) ) ;
#10803 = ORIENTED_EDGE ( 'NONE', *, *, #12185, .F. ) ;
#10804 = PLANE ( 'NONE',  #9515 ) ;
#10805 = EDGE_CURVE ( 'NONE', #7893, #17463, #9195, .T. ) ;
#10806 =( BOUNDED_CURVE ( )  B_SPLINE_CURVE ( 2, ( #4556, #18833, #17542, #10768, #1068 ),
 .UNSPECIFIED., .F., .T. ) 
 B_SPLINE_CURVE_WITH_KNOTS ( ( 3, 2, 3 ),
 ( 0.6333811345117427161, 0.6500000000000000222, 0.6577596748367573465 ),
 .UNSPECIFIED. ) 
 CURVE ( )  GEOMETRIC_REPRESENTATION_ITEM ( )  RATIONAL_B_SPLINE_CURVE ( ( 0.9660722070828660080, 0.9493985675960723292, 1.000000000000000000, 0.9763731969546250999, 0.9674132986343875196 ) ) 
 REPRESENTATION_ITEM ( '' )  );
#10807 = ADVANCED_FACE ( 'NONE', ( #9086 ), #19348, .F. ) ;
#10808 = EDGE_CURVE ( 'NONE', #17046, #279, #16918, .T. ) ;
#10809 = VERTEX_POINT ( 'NONE', #5776 ) ;
#10810 = DIRECTION ( 'NONE',  ( 1.000000000000000000, 0.000000000000000000, 0.000000000000000000 ) ) ;
#10811 = CARTESIAN_POINT ( 'NONE',  ( -3.350035803220276609, 49.20851703305431357, 93.38308880123798872 ) ) ;
#10812 = CARTESIAN_POINT ( 'NONE',  ( 5.008928291858447679, 51.78839635354462700, 75.50506468444432073 ) ) ;
#10813 = ORIENTED_EDGE ( 'NONE', *, *, #17950, .F. ) ;
#10814 = CARTESIAN_POINT ( 'NONE',  ( 4.394343283833276992, 39.11584570990505938, 92.75808880123797451 ) ) ;
#10815 = CARTESIAN_POINT ( 'NONE',  ( -5.171864905379679023, 50.90921633613218944, 79.44348587025405095 ) ) ;
#10816 = DIRECTION ( 'NONE',  ( 0.8660254037844395958, -0.4999999999999985012, 0.000000000000000000 ) ) ;
#10817 = VERTEX_POINT ( 'NONE', #12283 ) ;
#10818 = VECTOR ( 'NONE', #12436, 1000.000000000000000 ) ;
#10819 = CARTESIAN_POINT ( 'NONE',  ( 4.521197205061672442, 36.20397919953602184, 75.90366482745062626 ) ) ;
#10820 = DIRECTION ( 'NONE',  ( -1.000000000000000000, 1.110223024625156540E-16, -1.779391786395883043E-16 ) ) ;
#10821 = EDGE_CURVE ( 'NONE', #14218, #14373, #1597, .T. ) ;
#10822 = ORIENTED_EDGE ( 'NONE', *, *, #7074, .T. ) ;
#10823 = LINE ( 'NONE', #7612, #5419 ) ;
#10824 = CARTESIAN_POINT ( 'NONE',  ( 4.394343283833276992, 39.11584570990505938, 92.75808880123797451 ) ) ;
#10825 = AXIS2_PLACEMENT_3D ( 'NONE', #9761, #16248, #8263 ) ;
#10826 = VERTEX_POINT ( 'NONE', #3191 ) ;
#10827 = DIRECTION ( 'NONE',  ( 1.000000000000000000, -0.000000000000000000, -0.000000000000000000 ) ) ;
#10828 = CARTESIAN_POINT ( 'NONE',  ( 23.03948732994508575, 36.35905713404685002, 76.90433879953101837 ) ) ;
#10829 = CARTESIAN_POINT ( 'NONE',  ( 2.463659247115867146, 38.82793883177424732, 93.03246379782397923 ) ) ;
#10830 = CONTEXT_DEPENDENT_SHAPE_REPRESENTATION ( #3289, #7169 ) ;
#10831 = CARTESIAN_POINT ( 'NONE',  ( 5.228508048761829841, 37.45631306436156649, 75.98067903659783440 ) ) ;
#10832 = CARTESIAN_POINT ( 'NONE',  ( 5.644533139590786064, 37.00667393039697828, 75.97264893529829521 ) ) ;
#10833 = VECTOR ( 'NONE', #16348, 1000.000000000000000 ) ;
#10834 = PLANE ( 'NONE',  #12989 ) ;
#10835 = EDGE_LOOP ( 'NONE', ( #13653, #11763, #1951, #11637, #7632, #18716 ) ) ;
#10836 = CARTESIAN_POINT ( 'NONE',  ( 0.7278995231378414532, 52.96529355253956339, 75.36169494263242541 ) ) ;
#10837 = ORIENTED_EDGE ( 'NONE', *, *, #20250, .F. ) ;
#10838 = CARTESIAN_POINT ( 'NONE',  ( 6.467647404187965243, 50.71089930605690910, 75.49932683761802821 ) ) ;
#10839 = ADVANCED_FACE ( 'NONE', ( #9696 ), #19456, .F. ) ;
#10840 = CARTESIAN_POINT ( 'NONE',  ( -0.001710212166300070519, 52.34625406315150542, 75.41767803229005551 ) ) ;
#10841 = CARTESIAN_POINT ( 'NONE',  ( 1.352400422481993658, 50.46853102219002096, 91.97683880123797451 ) ) ;
#10842 = ORIENTED_EDGE ( 'NONE', *, *, #7390, .T. ) ;
#10843 = CARTESIAN_POINT ( 'NONE',  ( -4.151536175905484072, 36.67403323987894481, 75.43521673441158271 ) ) ;
#10844 = EDGE_CURVE ( 'NONE', #2871, #18295, #8295, .T. ) ;
#10845 = CARTESIAN_POINT ( 'NONE',  ( 5.807634474669838731, 51.19842427014940967, 79.54761434581399726 ) ) ;
#10846 = ORIENTED_EDGE ( 'NONE', *, *, #11977, .F. ) ;
#10847 = CARTESIAN_POINT ( 'NONE',  ( 5.706854332355044690, 51.27286650160559134, 79.54768974400036541 ) ) ;
#10848 = DIRECTION ( 'NONE',  ( -3.893792155548169402E-16, -7.183611964723547524E-17, 1.000000000000000000 ) ) ;
#10849 = CARTESIAN_POINT ( 'NONE',  ( 8.392716226808454749, 39.94722745792154939, 76.30598982719874357 ) ) ;
#10850 = CIRCLE ( 'NONE', #977, 8.199999999999995737 ) ;
#10851 = EDGE_CURVE ( 'NONE', #13249, #18186, #17565, .T. ) ;
#10852 = EDGE_LOOP ( 'NONE', ( #19839, #415, #17725, #1406 ) ) ;
#10853 = CARTESIAN_POINT ( 'NONE',  ( -4.853788242550845844, 37.19275855307111556, 77.90854597583356167 ) ) ;
#10854 = LINE ( 'NONE', #1362, #14516 ) ;
#10855 = CARTESIAN_POINT ( 'NONE',  ( -4.588881395441816835, 37.74767372618060080, 79.54736998457485697 ) ) ;
#10856 = CARTESIAN_POINT ( 'NONE',  ( -4.567115856812060670, 47.10047254335474065, 95.80496380123798872 ) ) ;
#10857 = FACE_OUTER_BOUND ( 'NONE', #19120, .T. ) ;
#10858 = CARTESIAN_POINT ( 'NONE',  ( 5.025485839985549319, 41.56218137147963887, 94.78933880294496817 ) ) ;
#10859 = CARTESIAN_POINT ( 'NONE',  ( 5.025485839985549319, 41.56218137147963887, 93.53933880294496817 ) ) ;
#10860 = CARTESIAN_POINT ( 'NONE',  ( -5.667418469993653396, 43.80274312437727247, 82.45433879953087342 ) ) ;
#10861 = CARTESIAN_POINT ( 'NONE',  ( 8.951691408152598228, 41.62251153713423690, 78.44085888008430629 ) ) ;
#10862 = CARTESIAN_POINT ( 'NONE',  ( -0.9369880318669705499, 52.97987177264234049, 77.93056416558285093 ) ) ;
#10863 = CARTESIAN_POINT ( 'NONE',  ( 0.3821786226492927541, 35.36301154328572949, 76.16022115247204738 ) ) ;
#10864 = DIRECTION ( 'NONE',  ( 1.540237394707284220E-16, 1.793354297423764243E-16, -1.000000000000000000 ) ) ;
#10865 = DIRECTION ( 'NONE',  ( -1.000000000000000000, 1.110223024625156540E-16, -1.779391786395883043E-16 ) ) ;
#10866 = CARTESIAN_POINT ( 'NONE',  ( -0.3080929418689875576, 37.85583172076933778, 91.35183880123798872 ) ) ;
#10867 = CARTESIAN_POINT ( 'NONE',  ( -8.170692237619920917, 42.45118346540571963, 79.33973788556694728 ) ) ;
#10868 = CARTESIAN_POINT ( 'NONE',  ( 5.500237024828340537, 36.90356520980568433, 77.71779572520892998 ) ) ;
#10869 = ORIENTED_EDGE ( 'NONE', *, *, #6737, .F. ) ;
#10870 = CARTESIAN_POINT ( 'NONE',  ( 11.22215374030650281, 42.76218137147968434, 78.80433879953099563 ) ) ;
#10871 = PLANE ( 'NONE',  #8752 ) ;
#10872 = DIRECTION ( 'NONE',  ( -1.193617070626243484E-16, -1.000000000000000000, -0.000000000000000000 ) ) ;
#10873 = CARTESIAN_POINT ( 'NONE',  ( 0.3281727876805012878, 52.35988662561128137, 78.59782856811732188 ) ) ;
#10874 = LINE ( 'NONE', #10771, #17244 ) ;
#10875 = VECTOR ( 'NONE', #10586, 1000.000000000000227 ) ;
#10876 = CARTESIAN_POINT ( 'NONE',  ( -1.477846259693493369, 50.16218137147969713, 77.55433879953099563 ) ) ;
#10877 = CYLINDRICAL_SURFACE ( 'NONE', #6048, 1.399999999999998579 ) ;
#10878 = VECTOR ( 'NONE', #12957, 1000.000000000000000 ) ;
#10879 = CARTESIAN_POINT ( 'NONE',  ( 6.828503391016846891, 43.33193468930419101, 91.50808880123798872 ) ) ;
#10880 = AXIS2_PLACEMENT_3D ( 'NONE', #13825, #7112, #10555 ) ;
#10881 = ADVANCED_FACE ( 'NONE', ( #2481 ), #12274, .F. ) ;
#10882 = CARTESIAN_POINT ( 'NONE',  ( 0.7879266358239551682, 52.35788869271873125, 78.84197803560836348 ) ) ;
#10883 = ORIENTED_EDGE ( 'NONE', *, *, #4669, .F. ) ;
#10884 = CARTESIAN_POINT ( 'NONE',  ( 5.936990147225109204, 51.10287444559717329, 77.01219674908871582 ) ) ;
#10885 = AXIS2_PLACEMENT_3D ( 'NONE', #19230, #19139, #13070 ) ;
#10886 = VERTEX_POINT ( 'NONE', #5444 ) ;
#10887 = DIRECTION ( 'NONE',  ( -4.142850521348543581E-16, 5.922860397471813007E-17, -1.000000000000000000 ) ) ;
#10888 = CARTESIAN_POINT ( 'NONE',  ( 3.948530577815480225, 39.69684013992245752, 90.96121380294498238 ) ) ;
#10889 = VERTEX_POINT ( 'NONE', #774 ) ;
#10890 = FACE_OUTER_BOUND ( 'NONE', #8332, .T. ) ;
#10892 = VECTOR ( 'NONE', #1327, 1000.000000000000000 ) ;
#10891 = DIRECTION ( 'NONE',  ( -1.000000000000000000, 0.000000000000000000, 0.000000000000000000 ) ) ;
#10893 = CIRCLE ( 'NONE', #13585, 0.5999999999999928724 ) ;
#10894 = DIRECTION ( 'NONE',  ( 1.239088197126290817E-16, 1.000000000000000000, 0.000000000000000000 ) ) ;
#10895 = CARTESIAN_POINT ( 'NONE',  ( 0.5221537403065008576, 44.16218137147968292, 80.45433879953087342 ) ) ;
#10896 = CARTESIAN_POINT ( 'NONE',  ( 0.7248365744723396231, 52.96455768829495270, 75.99814205791308552 ) ) ;
#10897 = CARTESIAN_POINT ( 'NONE',  ( 0.3821786226492926430, 35.36301154328572949, 76.86610350541323555 ) ) ;
#10898 = ORIENTED_EDGE ( 'NONE', *, *, #8373, .T. ) ;
#10899 = CARTESIAN_POINT ( 'NONE',  ( 0.5221537403065010796, 44.16218137147968292, 78.25433879953088478 ) ) ;
#10900 = ORIENTED_EDGE ( 'NONE', *, *, #2328, .F. ) ;
#10901 = CARTESIAN_POINT ( 'NONE',  ( 6.828503391016846891, 43.33193468930419101, 95.25808880123800293 ) ) ;
#10902 = AXIS2_PLACEMENT_3D ( 'NONE', #4300, #19294, #218 ) ;
#10903 = AXIS2_PLACEMENT_3D ( 'NONE', #14209, #17720, #1553 ) ;
#10904 = CARTESIAN_POINT ( 'NONE',  ( 5.568489401881125289, 48.03437091500646261, 95.41433880123797451 ) ) ;
#10905 = DIRECTION ( 'NONE',  ( 0.000000000000000000, -1.000000000000000000, -2.168404344970984808E-15 ) ) ;
#10906 = CARTESIAN_POINT ( 'NONE',  ( 0.5221537403065010796, 44.16218137147969003, 50.15433879953098995 ) ) ;
#10907 = CARTESIAN_POINT ( 'NONE',  ( 5.383107995780706645, 37.55798503218719020, 78.33046556645599878 ) ) ;
#10908 = AXIS2_PLACEMENT_3D ( 'NONE', #19979, #16814, #3923 ) ;
#10909 = ORIENTED_EDGE ( 'NONE', *, *, #2098, .F. ) ;
#10910 = CARTESIAN_POINT ( 'NONE',  ( 8.246890682022526065, 41.41102172004362814, 76.01662778496600481 ) ) ;
#10911 = ORIENTED_EDGE ( 'NONE', *, *, #16944, .T. ) ;
#10912 = CARTESIAN_POINT ( 'NONE',  ( -2.915357068909699478, 51.60185863777040538, 76.59793576264409865 ) ) ;
#10913 = ADVANCED_FACE ( 'NONE', ( #8976 ), #20726, .T. ) ;
#10914 = CARTESIAN_POINT ( 'NONE',  ( -3.350035803220276609, 49.20851703305431357, 94.63308880123798872 ) ) ;
#10915 = LINE ( 'NONE', #9519, #19328 ) ;
#10916 = ORIENTED_EDGE ( 'NONE', *, *, #18204, .T. ) ;
#10917 = CARTESIAN_POINT ( 'NONE',  ( -5.048916887735209080, 50.07712348856472317, 79.26884812577799266 ) ) ;
#10918 = DIRECTION ( 'NONE',  ( -3.211742425186504723E-16, 5.922860397471811774E-17, -1.000000000000000000 ) ) ;
#10919 = EDGE_LOOP ( 'NONE', ( #17581, #14105, #20306, #9319, #10842 ) ) ;
#10920 = CARTESIAN_POINT ( 'NONE',  ( -4.157944255866825145, 37.43340257241605684, 78.67445481091525039 ) ) ;
#10921 = CARTESIAN_POINT ( 'NONE',  ( -4.244931195431495219, 50.82465379583177878, 78.93669174070734584 ) ) ;
#10922 = ADVANCED_FACE ( 'NONE', ( #9079 ), #665, .F. ) ;
#10923 = VERTEX_POINT ( 'NONE', #20447 ) ;
#10924 = CARTESIAN_POINT ( 'NONE',  ( -5.917125461193805336, 40.64525615903904310, 76.16022115247204738 ) ) ;
#10925 = DIRECTION ( 'NONE',  ( -0.9534635866061452747, -0.3015081906286225522, -2.009271279954815797E-16 ) ) ;
#10926 = VERTEX_POINT ( 'NONE', #3955 ) ;
#10927 = PLANE ( 'NONE',  #909 ) ;
#10928 = CARTESIAN_POINT ( 'NONE',  ( 5.829886354652526137, 45.28396961230274087, 95.05433879953102405 ) ) ;
#10929 = CARTESIAN_POINT ( 'NONE',  ( 2.921181103050038086, 49.30691215337508737, 94.75121379782399345 ) ) ;
#10930 = CARTESIAN_POINT ( 'NONE',  ( 5.074636438210348821, 37.34636204506070811, 76.67247627436783830 ) ) ;
#10931 =( BOUNDED_CURVE ( )  B_SPLINE_CURVE ( 2, ( #15445, #5751, #11658 ),
 .UNSPECIFIED., .F., .F. ) 
 B_SPLINE_CURVE_WITH_KNOTS ( ( 3, 3 ),
 ( 0.1123202270280673071, 0.1128933701044576160 ),
 .UNSPECIFIED. ) 
 CURVE ( )  GEOMETRIC_REPRESENTATION_ITEM ( )  RATIONAL_B_SPLINE_CURVE ( ( 0.9672500519790907525, 0.9666242557201361052, 0.9660722070857192811 ) ) 
 REPRESENTATION_ITEM ( '' )  );
#10932 = LINE ( 'NONE', #2828, #20387 ) ;
#10933 = CARTESIAN_POINT ( 'NONE',  ( -7.567930892892213102, 42.78490342736719754, 76.47044134360902490 ) ) ;
#10934 = EDGE_LOOP ( 'NONE', ( #3891, #7413, #15133, #3224, #2867 ) ) ;
#10935 = CARTESIAN_POINT ( 'NONE',  ( 2.118098838249972804, 52.81625338523218716, 77.70152060498777757 ) ) ;
#10936 = ORIENTED_EDGE ( 'NONE', *, *, #13739, .F. ) ;
#10937 = CARTESIAN_POINT ( 'NONE',  ( 31.22215374030650281, 45.56218137147968861, 78.80433879953099563 ) ) ;
#10938 = CARTESIAN_POINT ( 'NONE',  ( 5.494509650718089055, 37.64638807017929167, 77.47236191065434241 ) ) ;
#10939 = CARTESIAN_POINT ( 'NONE',  ( 2.043125170982144745, 38.48583871533720213, 92.67996380123798872 ) ) ;
#10940 = CARTESIAN_POINT ( 'NONE',  ( -3.173569252698743348, 51.48240278743190146, 75.75534724892666816 ) ) ;
#10941 = VERTEX_POINT ( 'NONE', #20121 ) ;
#10942 = ORIENTED_EDGE ( 'NONE', *, *, #18320, .F. ) ;
#10943 = VECTOR ( 'NONE', #20411, 1000.000000000000000 ) ;
#10944 = CARTESIAN_POINT ( 'NONE',  ( -3.096437231170314330, 36.81950709836767999, 76.12177974158937843 ) ) ;
#10945 = CARTESIAN_POINT ( 'NONE',  ( 5.898472913175941024, 51.13132557482045826, 79.54598470662274678 ) ) ;
#10946 = CIRCLE ( 'NONE', #3448, 3.999999999999996447 ) ;
#10947 = ORIENTED_EDGE ( 'NONE', *, *, #19232, .T. ) ;
#10948 = CARTESIAN_POINT ( 'NONE',  ( 0.5221537403064990812, 39.96218137147968719, 92.45433879953097289 ) ) ;
#10949 = CARTESIAN_POINT ( 'NONE',  ( -7.723582874747324745, 47.23591325229828186, 77.58227997600145898 ) ) ;
#10950 = CARTESIAN_POINT ( 'NONE',  ( 5.220616844236031895, 45.87228208810806507, 91.54808879953097289 ) ) ;
#10951 = ORIENTED_EDGE ( 'NONE', *, *, #9829, .F. ) ;
#10952 = DIRECTION ( 'NONE',  ( -0.007885122365285377952, -0.9999689119394085113, -1.805443505845558427E-16 ) ) ;
#10953 = CARTESIAN_POINT ( 'NONE',  ( -6.856111849776215017, 40.77524371008118464, 79.32598559883581402 ) ) ;
#10954 = CARTESIAN_POINT ( 'NONE',  ( -1.477846259693489372, 50.16218137147969713, 50.55433879953100273 ) ) ;
#10955 = CARTESIAN_POINT ( 'NONE',  ( 1.352400422481993658, 50.46853102219002096, 90.72683880123797451 ) ) ;
#10956 = DIRECTION ( 'NONE',  ( 0.5773502691896226224, 0.5773502691896224004, -0.5773502691896322814 ) ) ;
#10957 = EDGE_CURVE ( 'NONE', #15270, #5478, #566, .T. ) ;
#10958 = ADVANCED_FACE ( 'NONE', ( #10478 ), #17514, .F. ) ;
#10959 = CARTESIAN_POINT ( 'NONE',  ( 5.655950003444441876, 37.76811099897118851, 78.37198585835440667 ) ) ;
#10960 = VECTOR ( 'NONE', #12072, 1000.000000000000000 ) ;
#10961 = CARTESIAN_POINT ( 'NONE',  ( 35.92215374030650565, 51.36218137147967866, 45.55433879953098852 ) ) ;
#10962 = EDGE_CURVE ( 'NONE', #4614, #7590, #20550, .T. ) ;
#10963 = LINE ( 'NONE', #1258, #2698 ) ;
#10964 = AXIS2_PLACEMENT_3D ( 'NONE', #5498, #7081, #13283 ) ;
#10965 = CARTESIAN_POINT ( 'NONE',  ( 2.522153740306511516, 50.16218137147969713, 51.55433879953100273 ) ) ;
#10966 = CARTESIAN_POINT ( 'NONE',  ( -1.477846259693492481, 49.81903562097207327, 69.15433879953098995 ) ) ;
#10967 = DIRECTION ( 'NONE',  ( -1.000000000000000000, 0.000000000000000000, 0.000000000000000000 ) ) ;
#10968 = CARTESIAN_POINT ( 'NONE',  ( 8.458367304687495647, 40.14398790315176058, 79.09910503406773330 ) ) ;
#10969 = DIRECTION ( 'NONE',  ( -0.5941461771851693774, -0.8043570849667760481, -2.357623395011396791E-16 ) ) ;
#10970 = ADVANCED_FACE ( 'NONE', ( #19368, #4479 ), #9395, .T. ) ;
#10971 = VERTEX_POINT ( 'NONE', #15880 ) ;
#10972 = CARTESIAN_POINT ( 'NONE',  ( 5.722153740306498371, 44.16218137147968292, 94.58161078214052964 ) ) ;
#10973 = MANIFOLD_SOLID_BREP ( 'Stock-MAS-160-1', #12560 ) ;
#10974 = CARTESIAN_POINT ( 'NONE',  ( 5.304793302263875354, 37.51082371353274425, 75.97198585835440099 ) ) ;
#10975 = EDGE_LOOP ( 'NONE', ( #5887, #11094, #5960, #17051 ) ) ;
#10976 = VECTOR ( 'NONE', #10628, 1000.000000000000000 ) ;
#10977 = CARTESIAN_POINT ( 'NONE',  ( -1.077846259693481246, 47.82824192744437397, 69.55433879953100984 ) ) ;
#10978 = CARTESIAN_POINT ( 'NONE',  ( -4.032917313034308116, 50.98063674598317618, 76.36012575652569012 ) ) ;
#10979 = CARTESIAN_POINT ( 'NONE',  ( 6.832223124813663340, 50.44160190723654580, 77.98033120372964788 ) ) ;
#10980 = CIRCLE ( 'NONE', #13328, 8.199999999999995737 ) ;
#10981 = CARTESIAN_POINT ( 'NONE',  ( 2.522153740306507963, 50.16218137147969713, 69.15433879953098995 ) ) ;
#10982 = CARTESIAN_POINT ( 'NONE',  ( 14.52215374030650175, 44.16218137147969003, 105.5543387995309956 ) ) ;
#10983 = LINE ( 'NONE', #3087, #20648 ) ;
#10984 = CARTESIAN_POINT ( 'NONE',  ( 5.347338439526899023, 50.79239070589999727, 75.97314036218482158 ) ) ;
#10985 = ORIENTED_EDGE ( 'NONE', *, *, #18068, .T. ) ;
#10986 = ADVANCED_FACE ( 'NONE', ( #2795 ), #15676, .T. ) ;
#10987 = CARTESIAN_POINT ( 'NONE',  ( 5.611423337425062385, 41.22389019960463230, 90.17996380123798872 ) ) ;
#10988 = AXIS2_PLACEMENT_3D ( 'NONE', #576, #7058, #2183 ) ;
#10989 = DIRECTION ( 'NONE',  ( -1.779391786395883536E-16, -5.922860397471806844E-17, 1.000000000000000000 ) ) ;
#10990 = VECTOR ( 'NONE', #17959, 1000.000000000000000 ) ;
#10991 = CARTESIAN_POINT ( 'NONE',  ( 10.77494014480653561, 42.96218137147968008, 69.40574467885102194 ) ) ;
#10992 = ORIENTED_EDGE ( 'NONE', *, *, #18444, .F. ) ;
#10993 = CARTESIAN_POINT ( 'NONE',  ( 27.03948732994508930, 36.35905713404685713, 76.90433879953101837 ) ) ;
#10994 = CARTESIAN_POINT ( 'NONE',  ( -3.943187491250720544, 40.73580453397070755, 91.89871380294498238 ) ) ;
#10995 = VERTEX_POINT ( 'NONE', #4577 ) ;
#10996 = DIRECTION ( 'NONE',  ( -1.540237394707284220E-16, -1.793354297423764243E-16, 1.000000000000000000 ) ) ;
#10997 = CARTESIAN_POINT ( 'NONE',  ( -2.077846259693550746, 39.65884927180063357, 94.16433879953098085 ) ) ;
#10998 = CARTESIAN_POINT ( 'NONE',  ( 5.755371611800503828, 51.23702874167446453, 77.28963291717792572 ) ) ;
#10999 = FACE_OUTER_BOUND ( 'NONE', #6811, .T. ) ;
#11000 = CARTESIAN_POINT ( 'NONE',  ( 0.8127483387853863261, 52.35242157994007783, 76.07424718102974737 ) ) ;
#11001 = CARTESIAN_POINT ( 'NONE',  ( -3.632788261743048253, 37.20487005735590458, 79.44037905412795908 ) ) ;
#11002 = ORIENTED_EDGE ( 'NONE', *, *, #1771, .T. ) ;
#11003 = CARTESIAN_POINT ( 'NONE',  ( 5.769916034762062829, 37.09626795672559041, 77.71701144737939160 ) ) ;
#11004 = VECTOR ( 'NONE', #339, 1000.000000000000000 ) ;
#11005 = ORIENTED_EDGE ( 'NONE', *, *, #20294, .T. ) ;
#11006 = CARTESIAN_POINT ( 'NONE',  ( -5.784195910403845176, 44.99242805365518194, 93.38308880123798872 ) ) ;
#11007 = CARTESIAN_POINT ( 'NONE',  ( -5.784195910403845176, 44.99242805365518194, 94.63308880123798872 ) ) ;
#11008 = DIRECTION ( 'NONE',  ( -0.000000000000000000, -0.000000000000000000, 1.000000000000000000 ) ) ;
#11009 = CARTESIAN_POINT ( 'NONE',  ( -4.622577041588897373, 46.56120873422322859, 95.06371379782397923 ) ) ;
#11010 = CARTESIAN_POINT ( 'NONE',  ( -7.357289765694363659, 41.91101321416308423, 78.82529883526802905 ) ) ;
#11011 = ORIENTED_EDGE ( 'NONE', *, *, #18213, .T. ) ;
#11012 = CARTESIAN_POINT ( 'NONE',  ( 2.263363662449209279, 49.77488197367684819, 94.28606768333811772 ) ) ;
#11013 = VERTEX_POINT ( 'NONE', #12475 ) ;
#11014 = AXIS2_PLACEMENT_3D ( 'NONE', #2904, #2690, #14385 ) ;
#11015 = CARTESIAN_POINT ( 'NONE',  ( -3.416741549526295163, 52.16336322705762996, 76.06019729239972094 ) ) ;
#11016 = CARTESIAN_POINT ( 'NONE',  ( 4.987494971863720927, 47.58855820898865829, 90.96121379953099506 ) ) ;
#11017 = CARTESIAN_POINT ( 'NONE',  ( -7.108943275890691638, 41.53885404143057514, 78.28419725522122974 ) ) ;
#11018 = VERTEX_POINT ( 'NONE', #18956 ) ;
#11019 = ADVANCED_FACE ( 'NONE', ( #1199, #7684 ), #15011, .T. ) ;
#11020 = CARTESIAN_POINT ( 'NONE',  ( -5.093619678490177272, 50.04518051096484754, 79.23104009678212378 ) ) ;
#11021 = FACE_OUTER_BOUND ( 'NONE', #5115, .T. ) ;
#11022 = CARTESIAN_POINT ( 'NONE',  ( 6.761578195034432248, 37.80487342938723572, 78.00072712051441215 ) ) ;
#11023 = CARTESIAN_POINT ( 'NONE',  ( -4.578222290571132724, 51.33341161403104280, 78.93596775356181183 ) ) ;
#11024 = ORIENTED_EDGE ( 'NONE', *, *, #3532, .F. ) ;
#11025 = DIRECTION ( 'NONE',  ( 1.540237394707284220E-16, 1.793354297423764243E-16, -1.000000000000000000 ) ) ;
#11026 = CARTESIAN_POINT ( 'NONE',  ( 5.568489401881125289, 48.03437091500646261, 90.57058880123798872 ) ) ;
#11027 = ORIENTED_EDGE ( 'NONE', *, *, #16773, .F. ) ;
#11028 = CARTESIAN_POINT ( 'NONE',  ( -5.103836094787935984, 44.83927886749827962, 92.45433879953098710 ) ) ;
#11029 = CARTESIAN_POINT ( 'NONE',  ( 4.374958955798271099, 39.84603773934203019, 95.05433879953099563 ) ) ;
#11030 = CARTESIAN_POINT ( 'NONE',  ( -1.876873622437039701, 39.01745058958429269, 94.12621379782397923 ) ) ;
#11031 = ADVANCED_FACE ( 'NONE', ( #6700 ), #13204, .T. ) ;
#11032 = CARTESIAN_POINT ( 'NONE',  ( -3.652148518534826138, 36.30515569394113129, 77.93013364623398331 ) ) ;
#11033 = CARTESIAN_POINT ( 'NONE',  ( 8.788905609664558582, 41.13463217212708400, 76.28640183395299346 ) ) ;
#11034 = CARTESIAN_POINT ( 'NONE',  ( -3.457680572327287649, 37.08634300271093309, 77.67016408458685817 ) ) ;
#11035 = ORIENTED_EDGE ( 'NONE', *, *, #8944, .T. ) ;
#11036 = CARTESIAN_POINT ( 'NONE',  ( 2.114701336805660414, 52.20152096667261787, 78.26636343789274974 ) ) ;
#11037 = CARTESIAN_POINT ( 'NONE',  ( 0.5221537403065010796, 44.16218137147968292, 78.13669174070733447 ) ) ;
#11038 = ORIENTED_EDGE ( 'NONE', *, *, #2339, .T. ) ;
#11039 = CARTESIAN_POINT ( 'NONE',  ( 1.456841371642047411, 39.25032235153333460, 92.45433879953097289 ) ) ;
#11040 = CARTESIAN_POINT ( 'NONE',  ( 30.92220646078100188, 45.56218137147968861, 62.80715055817104542 ) ) ;
#11041 = CARTESIAN_POINT ( 'NONE',  ( -2.416137431568557314, 39.07291177436112406, 91.27371380123798872 ) ) ;
#11042 = CYLINDRICAL_SURFACE ( 'NONE', #10183, 6.999999999999999112 ) ;
#11043 = ORIENTED_EDGE ( 'NONE', *, *, #17021, .F. ) ;
#11044 = EDGE_LOOP ( 'NONE', ( #20239, #19785, #13826, #3778 ) ) ;
#11045 = EDGE_CURVE ( 'NONE', #1084, #17463, #16607, .T. ) ;
#11046 = CARTESIAN_POINT ( 'NONE',  ( -3.274807807204083154, 36.95126225767872796, 75.71473766112499959 ) ) ;
#11047 = CARTESIAN_POINT ( 'NONE',  ( 8.333090968688148692, 41.66583349331221342, 78.92761653162175151 ) ) ;
#11048 = DIRECTION ( 'NONE',  ( 0.000000000000000000, -1.000000000000000000, 2.168404344970984413E-15 ) ) ;
#11049 = ORIENTED_EDGE ( 'NONE', *, *, #11554, .F. ) ;
#11050 = CARTESIAN_POINT ( 'NONE',  ( 6.545534159973747990, 50.65336749702785113, 77.68963291717794561 ) ) ;
#11051 = CARTESIAN_POINT ( 'NONE',  ( -3.154801521863568325, 47.83913663364971569, 83.28180655319408743 ) ) ;
#11052 = CARTESIAN_POINT ( 'NONE',  ( -3.467962453771610498, 40.50591351489412517, 92.25121379953098710 ) ) ;
#11053 = EDGE_LOOP ( 'NONE', ( #13460, #11202, #15495, #7989 ) ) ;
#11054 = CARTESIAN_POINT ( 'NONE',  ( 6.499036340715795390, 49.77623430136497262, 76.16185523003329649 ) ) ;
#11055 = CARTESIAN_POINT ( 'NONE',  ( -7.121200219685121624, 41.61353638602459171, 79.54638463348854316 ) ) ;
#11056 = CARTESIAN_POINT ( 'NONE',  ( -5.474757466566057218, 38.56948656142584753, 78.95744879387162030 ) ) ;
#11057 = CARTESIAN_POINT ( 'NONE',  ( -4.567115856812060670, 47.10047254335474065, 92.21121380123797451 ) ) ;
#11058 = SHAPE_REPRESENTATION_RELATIONSHIP ( 'NONE' , 'NONE' ,  #209, #11387 ) ;
#11059 = ADVANCED_FACE ( 'NONE', ( #8314 ), #13417, .F. ) ;
#11060 = CARTESIAN_POINT ( 'NONE',  ( -5.838428831739582492, 50.43291415881836315, 76.76022115247205591 ) ) ;
#11061 = ADVANCED_FACE ( 'NONE', ( #6914 ), #14691, .F. ) ;
#11062 = FACE_OUTER_BOUND ( 'NONE', #12933, .T. ) ;
#11063 = CARTESIAN_POINT ( 'NONE',  ( 8.644901377098815232, 43.03925179711409754, 75.45433879953088763 ) ) ;
#11064 = CARTESIAN_POINT ( 'NONE',  ( -0.1926216938105645149, 52.97400217050763160, 79.43762534667510522 ) ) ;
#11065 = EDGE_LOOP ( 'NONE', ( #8573, #6042, #1561, #19061, #8780, #10378, #20848, #2068, #2670, #362, #12449, #3504, #1101 ) ) ;
#11066 = CARTESIAN_POINT ( 'NONE',  ( -4.176781812633367785, 37.44206058802408421, 76.15041543488503351 ) ) ;
#11067 = DIRECTION ( 'NONE',  ( 0.3165065846431829311, 0.9485903129789527988, 2.188653791613874255E-16 ) ) ;
#11068 = EDGE_CURVE ( 'NONE', #20901, #19399, #4645, .T. ) ;
#11069 = CARTESIAN_POINT ( 'NONE',  ( -7.320717484398829633, 46.55579181444844750, 79.45433879953087342 ) ) ;
#11070 = CARTESIAN_POINT ( 'NONE',  ( -5.784195910403845176, 44.99242805365518194, 91.03933880123798872 ) ) ;
#11071 = EDGE_CURVE ( 'NONE', #8686, #1769, #2030, .T. ) ;
#11072 = ORIENTED_EDGE ( 'NONE', *, *, #13273, .F. ) ;
#11073 = EDGE_CURVE ( 'NONE', #17248, #17173, #20709, .T. ) ;
#11074 = ORIENTED_EDGE ( 'NONE', *, *, #6101, .T. ) ;
#11075 = PRODUCT_DEFINITION ( 'UNKNOWN', '', #5461, #14852 ) ;
#11076 = DIRECTION ( 'NONE',  ( -1.239088197126290817E-16, -1.000000000000000000, 0.000000000000000000 ) ) ;
#11077 = CARTESIAN_POINT ( 'NONE',  ( -3.874372605692205873, 36.46930367539203388, 79.33401574558745040 ) ) ;
#11078 = EDGE_CURVE ( 'NONE', #15788, #15252, #16188, .T. ) ;
#11079 = CARTESIAN_POINT ( 'NONE',  ( 23.03948732994508575, 45.16218137147969003, 76.90433879953101837 ) ) ;
#11080 = CARTESIAN_POINT ( 'NONE',  ( 1.256812508749381774, 49.74246873332880625, 91.11746379953096664 ) ) ;
#11081 = DIRECTION ( 'NONE',  ( 0.000000000000000000, 0.000000000000000000, -1.000000000000000000 ) ) ;
#11082 = CARTESIAN_POINT ( 'NONE',  ( 8.869748494521283888, 41.37692342661967615, 77.52492703482499792 ) ) ;
#11083 = CARTESIAN_POINT ( 'NONE',  ( 6.489427164124363046, 49.76997852774753994, 77.12327887040382279 ) ) ;
#11084 = LINE ( 'NONE', #16073, #6722 ) ;
#11085 = CARTESIAN_POINT ( 'NONE',  ( 5.245347708343344628, 50.86538805717837874, 76.02658503615866437 ) ) ;
#11086 = VERTEX_POINT ( 'NONE', #6489 ) ;
#11087 = PLANE ( 'NONE',  #9555 ) ;
#11088 = LINE ( 'NONE', #14368, #11279 ) ;
#11089 = CARTESIAN_POINT ( 'NONE',  ( -3.055718635266669647, 36.78391400955043622, 76.62933879953087057 ) ) ;
#11090 = ORIENTED_EDGE ( 'NONE', *, *, #5472, .T. ) ;
#11091 = CYLINDRICAL_SURFACE ( 'NONE', #9882, 1.399999999999998579 ) ;
#11092 = EDGE_CURVE ( 'NONE', #4079, #12581, #925, .T. ) ;
#11093 = CARTESIAN_POINT ( 'NONE',  ( 3.122153740306552905, 48.66551347115873227, 92.60183880294498238 ) ) ;
#11094 = ORIENTED_EDGE ( 'NONE', *, *, #7976, .F. ) ;
#11095 = DIRECTION ( 'NONE',  ( -1.540237394707283727E-16, -1.793354297423763257E-16, 1.000000000000000000 ) ) ;
#11096 = CARTESIAN_POINT ( 'NONE',  ( -0.8472276979131061481, 52.97793871905674479, 76.01337353251631157 ) ) ;
#11097 = DIRECTION ( 'NONE',  ( -0.5941461771851691553, -0.8043570849667760481, -2.357623395011396791E-16 ) ) ;
#11098 = DIRECTION ( 'NONE',  ( 0.000000000000000000, 0.000000000000000000, -1.000000000000000000 ) ) ;
#11099 = CARTESIAN_POINT ( 'NONE',  ( 0.8431453059911918624, 52.96362478046774669, 76.16511824318942558 ) ) ;
#11100 = EDGE_CURVE ( 'NONE', #8246, #13387, #2185, .T. ) ;
#11101 = CARTESIAN_POINT ( 'NONE',  ( 35.92215374030650565, 36.96218137147968719, 45.55433879953098852 ) ) ;
#11102 = ORIENTED_EDGE ( 'NONE', *, *, #2390, .F. ) ;
#11103 = DIRECTION ( 'NONE',  ( -1.540237394707284220E-16, -1.793354297423764243E-16, 1.000000000000000000 ) ) ;
#11104 = VERTEX_POINT ( 'NONE', #20096 ) ;
#11105 = DIRECTION ( 'NONE',  ( -0.009567942452863074584, 0.9999542261909885044, 1.778535306010356147E-16 ) ) ;
#11106 = CARTESIAN_POINT ( 'NONE',  ( -5.784195910403845176, 44.99242805365518194, 95.88308880123798872 ) ) ;
#11107 = CARTESIAN_POINT ( 'NONE',  ( 0.5186725038864670179, 52.36221944467538947, 75.97427063642290079 ) ) ;
#11108 = B_SPLINE_CURVE_WITH_KNOTS ( 'NONE', 3,
 ( #20432, #7344, #4250, #5749, #17037, #13735, #17240, #13836, #8957, #20535, #13950, #20315, #2563, #966, #12258 ),
 .UNSPECIFIED., .F., .F.,
 ( 4, 1, 1, 1, 1, 1, 1, 1, 1, 1, 1, 1, 4 ),
 ( 0.000000000000000000, 0.1267531625455885769, 0.2402085644777646467, 0.3404273024139109483, 0.4286057740769950719, 0.5026654758471001960, 0.5652545264784208934, 0.6141369997546152204, 0.6524264903941315863, 0.7200380101346053330, 0.7961149349448265466, 0.8886173437222998350, 0.9999999999999998890 ),
 .UNSPECIFIED. ) ;
#11109 = CARTESIAN_POINT ( 'NONE',  ( 0.5221537403065045213, 39.16218137147969003, 94.60386871425484401 ) ) ;
#11110 = CARTESIAN_POINT ( 'NONE',  ( -7.876934599565286632, 41.52403546573567183, 78.93589458924091673 ) ) ;
#11111 = ORIENTED_EDGE ( 'NONE', *, *, #11448, .F. ) ;
#11112 = DIRECTION ( 'NONE',  ( -1.000000000000000000, 1.110223024625156540E-16, -1.779391786395883043E-16 ) ) ;
#11113 = VERTEX_POINT ( 'NONE', #15437 ) ;
#11114 = VECTOR ( 'NONE', #10827, 1000.000000000000000 ) ;
#11115 = CARTESIAN_POINT ( 'NONE',  ( -3.013002030064880987, 51.53208512353911175, 75.97742918362793318 ) ) ;
#11116 = CARTESIAN_POINT ( 'NONE',  ( -0.3080929418689875576, 37.85583172076933778, 93.85183880123797451 ) ) ;
#11117 = CARTESIAN_POINT ( 'NONE',  ( -7.090928860711239068, 41.48188680325438327, 78.43135113490271237 ) ) ;
#11118 = ORIENTED_EDGE ( 'NONE', *, *, #7074, .F. ) ;
#11119 = CARTESIAN_POINT ( 'NONE',  ( -5.838428831739585156, 50.43291415881836315, 78.10580938776615767 ) ) ;
#11120 = CARTESIAN_POINT ( 'NONE',  ( 6.539349088566551949, 37.64607664623218142, 78.24541959536460922 ) ) ;
#11121 = DIRECTION ( 'NONE',  ( 5.626130192357176673E-16, 1.809130530872730902E-30, -1.000000000000000000 ) ) ;
#11122 = CARTESIAN_POINT ( 'NONE',  ( 2.522153740306498193, 49.81903562097208038, 123.5543387995310098 ) ) ;
#11123 = ORIENTED_EDGE ( 'NONE', *, *, #9534, .F. ) ;
#11124 = CARTESIAN_POINT ( 'NONE',  ( -4.826915440150258974, 45.06110468568228100, 92.55433879953100984 ) ) ;
#11125 = CARTESIAN_POINT ( 'NONE',  ( -0.9988176903691428077, 49.83852402762217082, 92.05496380123798872 ) ) ;
#11126 = ORIENTED_EDGE ( 'NONE', *, *, #9829, .T. ) ;
#11127 = CARTESIAN_POINT ( 'NONE',  ( 4.751063331615088536, 51.97887081224218520, 77.86982703766624070 ) ) ;
#11128 = CARTESIAN_POINT ( 'NONE',  ( 5.892585134170466254, 42.58711300521386534, 95.05433879953099563 ) ) ;
#11129 = LINE ( 'NONE', #3141, #19035 ) ;
#11130 = CARTESIAN_POINT ( 'NONE',  ( 5.666884522201895535, 41.76315400873614436, 93.18871379782397923 ) ) ;
#11131 = AXIS2_PLACEMENT_3D ( 'NONE', #13654, #2059, #18227 ) ;
#11132 = B_SPLINE_CURVE_WITH_KNOTS ( 'NONE', 3,
 ( #16855, #11759, #5458, #14832, #2273, #6740, #7160, #13662, #13350, #8455, #249, #6319, #13141, #20990, #8140, #2204, #20271, #16991, #12209, #18692, #2528, #15185, #601, #13583, #13900, #20385, #20064 ),
 .UNSPECIFIED., .F., .F.,
 ( 4, 1, 1, 1, 1, 1, 1, 1, 1, 1, 1, 1, 1, 1, 1, 1, 1, 1, 1, 1, 1, 1, 1, 1, 4 ),
 ( 0.000000000000000000, 0.04692756115915790172, 0.09175764483083305445, 0.1348320239538815524, 0.1755606184341063081, 0.2149124488236470176, 0.2520401868719510108, 0.2875439711136699161, 0.3211732624427411364, 0.3845494416143411254, 0.4434775415870848558, 0.4991878644837567380, 0.5522905917841786083, 0.6030460594100006677, 0.6509449284921694501, 0.6968976034913704209, 0.7406443924834601455, 0.7634319837341128068, 0.7890572409307390345, 0.8171397283500007047, 0.8480511511928767732, 0.8815178987434894031, 0.9182285974223420855, 0.9576130192529551666, 1.000000000000000000 ),
 .UNSPECIFIED. ) ;
#11133 = CARTESIAN_POINT ( 'NONE',  ( 5.075898477934015496, 37.34726385244101721, 76.52220546472133833 ) ) ;
#11134 = CARTESIAN_POINT ( 'NONE',  ( 8.207311740369052089, 47.02196222218739763, 75.43669174070734584 ) ) ;
#11135 = CARTESIAN_POINT ( 'NONE',  ( -3.053961058146955398, 36.78813166039994798, 76.77671532909576513 ) ) ;
#11136 = VERTEX_POINT ( 'NONE', #4143 ) ;
#11137 = CARTESIAN_POINT ( 'NONE',  ( 2.089542904467925677, 52.95439430598839436, 78.73916595950259989 ) ) ;
#11138 = VERTEX_POINT ( 'NONE', #2456 ) ;
#11139 = CARTESIAN_POINT ( 'NONE',  ( -8.190409139795066906, 42.92474528817020740, 76.06610350541322418 ) ) ;
#11140 = DIRECTION ( 'NONE',  ( 0.3165065846431827645, 0.9485903129789529098, 0.000000000000000000 ) ) ;
#11141 = CARTESIAN_POINT ( 'NONE',  ( 9.263154249150899133, 42.55598543044034443, 79.20437336408532758 ) ) ;
#11142 = CARTESIAN_POINT ( 'NONE',  ( 8.097263698133225773, 41.42615553683592111, 79.54516904849367620 ) ) ;
#11143 = VERTEX_POINT ( 'NONE', #7338 ) ;
#11144 = CARTESIAN_POINT ( 'NONE',  ( -5.784195910403845176, 44.99242805365518194, 93.53933880123797451 ) ) ;
#11145 = ORIENTED_EDGE ( 'NONE', *, *, #13409, .F. ) ;
#11146 = STYLED_ITEM ( 'NONE', ( #17758 ), #11462 ) ;
#11147 = CARTESIAN_POINT ( 'NONE',  ( -3.560029042603979565, 37.16194369485645410, 75.49480657079904233 ) ) ;
#11148 = CARTESIAN_POINT ( 'NONE',  ( -4.718161399584269056, 37.09257646755418847, 75.97198585835440099 ) ) ;
#11149 = DIRECTION ( 'NONE',  ( -1.084202172485505420E-16, -1.000000000000000000, 0.000000000000000000 ) ) ;
#11150 = ORIENTED_EDGE ( 'NONE', *, *, #13298, .F. ) ;
#11151 = CARTESIAN_POINT ( 'NONE',  ( -4.686954935604244810, 37.06952550968518523, 77.27854074750605662 ) ) ;
#11152 = CARTESIAN_POINT ( 'NONE',  ( 8.791848479292760032, 41.14345213909496835, 77.32915800260404637 ) ) ;
#11153 = CARTESIAN_POINT ( 'NONE',  ( -4.812088799398938299, 42.22067586467031930, 91.31371379782397923 ) ) ;
#11154 = VERTEX_POINT ( 'NONE', #5634 ) ;
#11155 = CARTESIAN_POINT ( 'NONE',  ( 8.550006361060139781, 45.88717064157471270, 78.74480812004853192 ) ) ;
#11156 = DIRECTION ( 'NONE',  ( 1.334402673828313339E-16, 1.871524341742854397E-32, -1.000000000000000000 ) ) ;
#11157 = CARTESIAN_POINT ( 'NONE',  ( 2.722153740306517911, 47.73989013547934945, 56.15433879953099705 ) ) ;
#11158 = CARTESIAN_POINT ( 'NONE',  ( -2.416137431568557314, 39.07291177436112406, 93.77371380123797451 ) ) ;
#11159 = AXIS2_PLACEMENT_3D ( 'NONE', #17031, #533, #2033 ) ;
#11160 = EDGE_CURVE ( 'NONE', #14970, #19160, #13940, .T. ) ;
#11161 = CARTESIAN_POINT ( 'NONE',  ( 2.122153740306511605, 50.16218137147969713, 61.55433879953100273 ) ) ;
#11162 = CARTESIAN_POINT ( 'NONE',  ( 0.3498111802063197939, 52.96792241217284669, 77.07502437766733294 ) ) ;
#11163 = B_SPLINE_CURVE_WITH_KNOTS ( 'NONE', 3,
 ( #4116, #16896, #12332, #4224, #5715, #1049, #830, #20073, #8814, #2430, #17114, #12021, #10646, #10750, #14023, #18814 ),
 .UNSPECIFIED., .F., .F.,
 ( 4, 2, 2, 2, 2, 2, 2, 4 ),
 ( 0.000000000000000000, 0.0002724318156510209619, 0.0005448636313020419238, 0.001089727262604055225, 0.001362159078255057105, 0.001634590893906058984, 0.001907022709557060864, 0.002179454525208062744 ),
 .UNSPECIFIED. ) ;
#11164 = CARTESIAN_POINT ( 'NONE',  ( 0.5221537403065019678, 44.16218137147968292, 72.45433879953087342 ) ) ;
#11165 = CARTESIAN_POINT ( 'NONE',  ( -0.9143118842621357212, 52.21725223193028853, 78.68934297065942474 ) ) ;
#11166 = ORIENTED_EDGE ( 'NONE', *, *, #8459, .F. ) ;
#11167 = DIRECTION ( 'NONE',  ( 0.5773502691896259531, 0.5773502691896257311, -0.5773502691896256200 ) ) ;
#11168 = DIRECTION ( 'NONE',  ( 1.193617070626243484E-16, 1.000000000000000000, 0.000000000000000000 ) ) ;
#11169 = CARTESIAN_POINT ( 'NONE',  ( 0.6854345734903630749, 52.36071088544267127, 75.98019728166023867 ) ) ;
#11170 = CARTESIAN_POINT ( 'NONE',  ( 1.328797878535935784, 52.92566332880988966, 79.46664029610046498 ) ) ;
#11171 = CIRCLE ( 'NONE', #7051, 0.9921021478795063464 ) ;
#11172 = ORIENTED_EDGE ( 'NONE', *, *, #6139, .F. ) ;
#11173 = EDGE_CURVE ( 'NONE', #2743, #1145, #15224, .T. ) ;
#11174 = VERTEX_POINT ( 'NONE', #16716 ) ;
#11175 = CARTESIAN_POINT ( 'NONE',  ( 9.317552545512265638, 42.71902057559893962, 75.91044101036179370 ) ) ;
#11176 = CARTESIAN_POINT ( 'NONE',  ( 2.337612517491833852, 49.93701999136722947, 72.45433879953087342 ) ) ;
#11177 = CARTESIAN_POINT ( 'NONE',  ( 6.873747143562635387, 50.41092978727617435, 78.08828162113617566 ) ) ;
#11179 = ADVANCED_FACE ( 'NONE', ( #20202 ), #9092, .F. ) ;
#11178 = CARTESIAN_POINT ( 'NONE',  ( -4.677846259693498432, 44.16218137147969003, 93.95661078214054385 ) ) ;
#11180 = DIRECTION ( 'NONE',  ( -1.540237394707283727E-16, -1.793354297423763257E-16, 1.000000000000000000 ) ) ;
#11181 = DIRECTION ( 'NONE',  ( 0.3014524538335020543, -0.9532873293559830374, -0.01922721423134257299 ) ) ;
#11182 = CARTESIAN_POINT ( 'NONE',  ( 6.295211134694258526, 49.91343808518868741, 77.55733179791843668 ) ) ;
#11183 = DIRECTION ( 'NONE',  ( -1.779391786395883536E-16, -5.922860397471806844E-17, 1.000000000000000000 ) ) ;
#11184 = ADVANCED_FACE ( 'NONE', ( #17028 ), #18298, .T. ) ;
#11185 = VECTOR ( 'NONE', #10801, 1000.000000000000114 ) ;
#11186 = CARTESIAN_POINT ( 'NONE',  ( -4.877143884790711148, 38.14601692126417731, 79.49842882144521639 ) ) ;
#11187 = CARTESIAN_POINT ( 'NONE',  ( 0.7560837815594079192, 52.35885938535841433, 78.87528329032154772 ) ) ;
#11188 = ADVANCED_FACE ( 'NONE', ( #959 ), #3718, .F. ) ;
#11189 = CARTESIAN_POINT ( 'NONE',  ( -3.156842967632347730, 36.83372846983282045, 77.40205577532607606 ) ) ;
#11190 = ORIENTED_EDGE ( 'NONE', *, *, #13078, .F. ) ;
#11191 = DIRECTION ( 'NONE',  ( 0.9485903129789495791, -0.3165065846431930341, 8.934458285744763183E-17 ) ) ;
#11192 = CARTESIAN_POINT ( 'NONE',  ( 8.848467398349676216, 41.31314263134580500, 75.36050707951255845 ) ) ;
#11193 = VERTEX_POINT ( 'NONE', #10239 ) ;
#11194 = VECTOR ( 'NONE', #15748, 1000.000000000000114 ) ;
#11195 = CARTESIAN_POINT ( 'NONE',  ( 6.882736312352589536, 37.89144858414100270, 76.69330938776616335 ) ) ;
#11196 = CARTESIAN_POINT ( 'NONE',  ( 8.985665979147935190, 41.72433548171385098, 78.13399373581940210 ) ) ;
#11197 = FACE_OUTER_BOUND ( 'NONE', #16409, .T. ) ;
#11198 = DIRECTION ( 'NONE',  ( -0.5813877811927011807, 0.8136266022444372803, 5.636455622144619183E-17 ) ) ;
#11199 = ORIENTED_EDGE ( 'NONE', *, *, #14580, .F. ) ;
#11200 = CARTESIAN_POINT ( 'NONE',  ( 5.544276951911417228, 50.64433212932689088, 72.45433879953087342 ) ) ;
#11201 = AXIS2_PLACEMENT_3D ( 'NONE', #18714, #2649, #7215 ) ;
#11202 = ORIENTED_EDGE ( 'NONE', *, *, #11859, .T. ) ;
#11203 = CARTESIAN_POINT ( 'NONE',  ( -5.154188915835984375, 42.64120994080404614, 95.96121380123798872 ) ) ;
#11204 = EDGE_CURVE ( 'NONE', #17246, #5430, #2139, .T. ) ;
#11205 = VECTOR ( 'NONE', #17241, 1000.000000000000000 ) ;
#11206 = CARTESIAN_POINT ( 'NONE',  ( 5.568489401881125289, 48.03437091500646261, 94.16433880123797451 ) ) ;
#11207 = CARTESIAN_POINT ( 'NONE',  ( -7.367656984315425817, 48.05973018190410073, 78.78375056423675460 ) ) ;
#11208 = CARTESIAN_POINT ( 'NONE',  ( 24.43948732994508077, 36.35905713404685002, 76.90433879953101837 ) ) ;
#11209 = EDGE_CURVE ( 'NONE', #2898, #5606, #15334, .T. ) ;
#11210 = FACE_OUTER_BOUND ( 'NONE', #2840, .T. ) ;
#11211 = VECTOR ( 'NONE', #12320, 1000.000000000000000 ) ;
#11212 = ORIENTED_EDGE ( 'NONE', *, *, #13910, .F. ) ;
#11213 = ADVANCED_FACE ( 'NONE', ( #747 ), #15120, .T. ) ;
#11214 = CARTESIAN_POINT ( 'NONE',  ( 4.890314246961300348, 51.87601177044496836, 77.76130678786321937 ) ) ;
#11215 = EDGE_CURVE ( 'NONE', #12777, #20326, #13510, .T. ) ;
#11216 = ORIENTED_EDGE ( 'NONE', *, *, #12621, .F. ) ;
#11217 = VECTOR ( 'NONE', #15067, 1000.000000000000000 ) ;
#11218 = CARTESIAN_POINT ( 'NONE',  ( -3.448085832972781262, 52.14096574969422448, 75.97742918362793318 ) ) ;
#11219 = VECTOR ( 'NONE', #18388, 1000.000000000000000 ) ;
#11220 = CARTESIAN_POINT ( 'NONE',  ( 5.611423337425062385, 41.22389019960463230, 95.33621380123798872 ) ) ;
#11221 = CARTESIAN_POINT ( 'NONE',  ( -7.789419058798823237, 41.24013430743122655, 78.49688471925094291 ) ) ;
#11222 = VERTEX_POINT ( 'NONE', #11933 ) ;
#11223 = CARTESIAN_POINT ( 'NONE',  ( 1.369964938772391561, 52.31939965602356324, 76.79052535208408869 ) ) ;
#11224 = CARTESIAN_POINT ( 'NONE',  ( 5.202885763635528349, 50.89499265101085967, 76.90580938776616904 ) ) ;
#11225 = CARTESIAN_POINT ( 'NONE',  ( 4.643940233704298315, 36.29168687389493897, 75.71841013695411959 ) ) ;
#11226 = CARTESIAN_POINT ( 'NONE',  ( 2.196093689222912371, 38.51591816243362842, 95.05433879953096721 ) ) ;
#11227 = FACE_OUTER_BOUND ( 'NONE', #20165, .T. ) ;
#11228 = ORIENTED_EDGE ( 'NONE', *, *, #19507, .F. ) ;
#11229 = VECTOR ( 'NONE', #1437, 1000.000000000000227 ) ;
#11230 = CARTESIAN_POINT ( 'NONE',  ( 6.691294758883309157, 37.75465145915448062, 79.45433879953087342 ) ) ;
#11231 = VECTOR ( 'NONE', #9207, 1000.000000000000114 ) ;
#11232 = FACE_OUTER_BOUND ( 'NONE', #7191, .T. ) ;
#11233 = VERTEX_POINT ( 'NONE', #18410 ) ;
#11234 = CARTESIAN_POINT ( 'NONE',  ( 4.791956560326987358, 51.94866463147243962, 77.83360891957636341 ) ) ;
#11235 = CARTESIAN_POINT ( 'NONE',  ( 3.321299285246416488, 39.00526458700550592, 95.05433879953096721 ) ) ;
#11236 = AXIS2_PLACEMENT_3D ( 'NONE', #19609, #19298, #5032 ) ;
#11237 = CARTESIAN_POINT ( 'NONE',  ( 5.848951923618479931, 37.15274410921379911, 77.37492703482499223 ) ) ;
#11238 = CARTESIAN_POINT ( 'NONE',  ( -4.007890887056448470, 40.01116025973682611, 91.54808879782400766 ) ) ;
#11239 = CIRCLE ( 'NONE', #5801, 0.9921021478795020165 ) ;
#11240 = CARTESIAN_POINT ( 'NONE',  ( 0.2541436421823717873, 38.02374091943176637, 91.54808879782400766 ) ) ;
#11241 = CARTESIAN_POINT ( 'NONE',  ( 11.22215374030649926, 45.56218137147968861, 70.80574467885102763 ) ) ;
#11242 = CARTESIAN_POINT ( 'NONE',  ( 5.889143815203415677, 51.13821660369377753, 76.04053158567903381 ) ) ;
#11243 = ORIENTED_EDGE ( 'NONE', *, *, #2328, .T. ) ;
#11244 = EDGE_CURVE ( 'NONE', #18543, #19191, #3829, .T. ) ;
#11245 = CARTESIAN_POINT ( 'NONE',  ( 2.111809426605781859, 52.81745860575872342, 77.55799709713352286 ) ) ;
#11246 = AXIS2_PLACEMENT_3D ( 'NONE', #10876, #12359, #20627 ) ;
#11247 = ORIENTED_EDGE ( 'NONE', *, *, #6604, .F. ) ;
#11248 = PLANE ( 'NONE',  #10903 ) ;
#11249 = CARTESIAN_POINT ( 'NONE',  ( -5.835824771109036746, 39.98772221508849611, 75.45433879953087342 ) ) ;
#11250 = FACE_OUTER_BOUND ( 'NONE', #2036, .T. ) ;
#11251 = B_SPLINE_SURFACE_WITH_KNOTS ( 'NONE', 3, 1, ( 
 ( #2387, #7050 ),
 ( #18449, #15376 ),
 ( #7491, #8674 ),
 ( #10603, #13551 ),
 ( #16958, #684 ),
 ( #20029, #20463 ),
 ( #790, #12179 ),
 ( #15155, #7271 ),
 ( #5460, #18772 ),
 ( #7163, #568 ),
 ( #20136, #5571 ),
 ( #10388, #4187 ),
 ( #13766, #2499 ),
 ( #8991, #16857 ),
 ( #890, #12394 ) ),
 .UNSPECIFIED., .F., .F., .F.,
 ( 4, 1, 1, 1, 1, 1, 1, 1, 1, 1, 1, 1, 4 ),
 ( 2, 2 ),
 ( 0.000000000000000000, 0.07527217715292475186, 0.1459465445934834404, 0.2117756949130734923, 0.2766029815265222958, 0.3381147468631120478, 0.3951637252042238257, 0.4534551218168583753, 0.5124046679576552688, 0.5890284689491043224, 0.6947781202056673155, 0.8321371544603952675, 0.9999999999999998890 ),
 ( 0.000000000000000000, 1.000000000000000000 ),
 .UNSPECIFIED. ) ;
#11252 = CARTESIAN_POINT ( 'NONE',  ( 7.928945443998646425, 40.92169505128364904, 79.45050910333212357 ) ) ;
#11253 = ORIENTED_EDGE ( 'NONE', *, *, #14917, .T. ) ;
#11254 = CARTESIAN_POINT ( 'NONE',  ( 5.709672981839667649, 51.27078447877342882, 77.95044976498417100 ) ) ;
#11255 = VERTEX_POINT ( 'NONE', #3930 ) ;
#11256 = CIRCLE ( 'NONE', #17688, 6.200000000000000178 ) ;
#11257 = CARTESIAN_POINT ( 'NONE',  ( -7.896563877726270775, 41.59953023782934878, 78.92964143347573724 ) ) ;
#11258 = DIRECTION ( 'NONE',  ( 1.540237394707284220E-16, 1.793354297423764243E-16, -1.000000000000000000 ) ) ;
#11259 = CARTESIAN_POINT ( 'NONE',  ( -6.721143750142749340, 40.31838871648160705, 78.26846280200385308 ) ) ;
#11260 = EDGE_LOOP ( 'NONE', ( #19999, #11422, #6325, #6644 ) ) ;
#11261 = CARTESIAN_POINT ( 'NONE',  ( -4.159002695544564254, 37.45430957594182786, 77.01245883157920957 ) ) ;
#11262 = CARTESIAN_POINT ( 'NONE',  ( -6.920047200808406629, 40.71838479833773050, 79.30581651637976393 ) ) ;
#11263 = CARTESIAN_POINT ( 'NONE',  ( -4.622577041588895597, 46.56120873422322859, 91.15746379782397923 ) ) ;
#11264 = ORIENTED_EDGE ( 'NONE', *, *, #9217, .T. ) ;
#11265 = DIRECTION ( 'NONE',  ( 1.000000000000000000, 1.402518428993831676E-16, 1.621236893436268400E-16 ) ) ;
#11266 = CARTESIAN_POINT ( 'NONE',  ( 5.457062992516449107, 50.71104673348453673, 78.93032258866925588 ) ) ;
#11267 = CARTESIAN_POINT ( 'NONE',  ( 6.375360725391126415, 38.41906761359206968, 75.91875917877068503 ) ) ;
#11268 = CARTESIAN_POINT ( 'NONE',  ( -0.9988176903691428077, 49.83852402762217082, 92.05496380123798872 ) ) ;
#11269 = EDGE_CURVE ( 'NONE', #19301, #11113, #12041, .T. ) ;
#11270 = CARTESIAN_POINT ( 'NONE',  ( -2.939085670389443905, 51.59587639763223166, 72.45433879953087342 ) ) ;
#11271 = CARTESIAN_POINT ( 'NONE',  ( 0.4452092196042181649, 52.34431542127848047, 76.95466777776533718 ) ) ;
#11272 = CARTESIAN_POINT ( 'NONE',  ( 2.122153740306512937, 49.76218137147969856, 53.55433879953100273 ) ) ;
#11273 = DIRECTION ( 'NONE',  ( -0.000000000000000000, -0.000000000000000000, 1.000000000000000000 ) ) ;
#11274 = ORIENTED_EDGE ( 'NONE', *, *, #14826, .F. ) ;
#11275 = DIRECTION ( 'NONE',  ( -1.110223024625156540E-16, -1.000000000000000000, -5.922860397471808077E-17 ) ) ;
#11276 = CARTESIAN_POINT ( 'NONE',  ( 9.351996896326966180, 42.82225248009945773, 76.45750776978282204 ) ) ;
#11277 = CARTESIAN_POINT ( 'NONE',  ( 0.8438208634514194895, 52.35586981924091532, 76.28587743965509560 ) ) ;
#11278 = CARTESIAN_POINT ( 'NONE',  ( 0.5221537403065118488, 48.16218137147969003, 45.55433879953100273 ) ) ;
#11279 = VECTOR ( 'NONE', #18943, 1000.000000000000000 ) ;
#11280 = ORIENTED_EDGE ( 'NONE', *, *, #18743, .T. ) ;
#11281 = ORIENTED_EDGE ( 'NONE', *, *, #15920, .F. ) ;
#11282 = EDGE_CURVE ( 'NONE', #6129, #15829, #10454, .T. ) ;
#11283 = DIRECTION ( 'NONE',  ( -1.621236893436268647E-16, -2.273814620809075225E-32, 1.000000000000000000 ) ) ;
#11284 = CARTESIAN_POINT ( 'NONE',  ( -4.463792963332828378, 40.72925446781975722, 72.45432679953087529 ) ) ;
#11285 = CARTESIAN_POINT ( 'NONE',  ( 6.903329084842819263, 50.38907879888579089, 78.20944795639196911 ) ) ;
#11286 = DIRECTION ( 'NONE',  ( -1.779391786395883536E-16, -5.922860397471806844E-17, 1.000000000000000000 ) ) ;
#11287 = CARTESIAN_POINT ( 'NONE',  ( -3.147842262194972207, 36.82924344237826375, 75.96820239334293490 ) ) ;
#11288 = AXIS2_PLACEMENT_3D ( 'NONE', #3349, #17822, #5041 ) ;
#11289 = FACE_OUTER_BOUND ( 'NONE', #11380, .T. ) ;
#11290 = DIRECTION ( 'NONE',  ( -0.007885122365275663500, -0.9999689119394085113, -1.805443505845543142E-16 ) ) ;
#11291 = CARTESIAN_POINT ( 'NONE',  ( 0.3201111382462866750, 51.36399839264385037, 77.76169174070734869 ) ) ;
#11292 = VECTOR ( 'NONE', #9575, 1000.000000000000000 ) ;
#11293 = EDGE_CURVE ( 'NONE', #20036, #2288, #14837, .T. ) ;
#11294 = EDGE_CURVE ( 'NONE', #16713, #14953, #4346, .T. ) ;
#11295 = VERTEX_POINT ( 'NONE', #6259 ) ;
#11296 = CARTESIAN_POINT ( 'NONE',  ( 0.5221537403065010796, 44.16218137147969003, 77.84651775085080772 ) ) ;
#11297 = ORIENTED_EDGE ( 'NONE', *, *, #10316, .F. ) ;
#11298 = CARTESIAN_POINT ( 'NONE',  ( 0.5221537403065048544, 39.16218137147969003, 93.66636871766883132 ) ) ;
#11299 = CARTESIAN_POINT ( 'NONE',  ( 5.831313177393474767, 37.14014010695713353, 78.35708441643889444 ) ) ;
#11300 = VECTOR ( 'NONE', #6147, 1000.000000000000000 ) ;
#11301 = CARTESIAN_POINT ( 'NONE',  ( 30.92220646078100188, 42.96218137147968008, 61.40715055817103263 ) ) ;
#11302 = VECTOR ( 'NONE', #7038, 1000.000000000000000 ) ;
#11303 = CARTESIAN_POINT ( 'NONE',  ( 9.054037327392332912, 41.92924874979977545, 78.13567616980381558 ) ) ;
#11304 = VERTEX_POINT ( 'NONE', #7661 ) ;
#11305 = CARTESIAN_POINT ( 'NONE',  ( -0.4710197511697722383, 52.21577876075154734, 75.60318094692254931 ) ) ;
#11306 = CARTESIAN_POINT ( 'NONE',  ( 0.07355455234133151388, 52.20946254203077075, 79.50648293536016809 ) ) ;
#11307 = CARTESIAN_POINT ( 'NONE',  ( 2.246318977524931260, 38.35943151540528362, 72.45433879953087342 ) ) ;
#11308 = DIRECTION ( 'NONE',  ( 1.193617070626243484E-16, 1.000000000000000000, 0.000000000000000000 ) ) ;
#11309 = CARTESIAN_POINT ( 'NONE',  ( 8.869748494521283888, 41.37692342661967615, 77.52492703482499792 ) ) ;
#11310 = ORIENTED_EDGE ( 'NONE', *, *, #18857, .T. ) ;
#11311 = CARTESIAN_POINT ( 'NONE',  ( 8.374986225289852371, 41.81414519758808979, 76.31823237213514233 ) ) ;
#11312 = EDGE_LOOP ( 'NONE', ( #15078, #16937, #4863, #4032, #19702, #14946, #4291, #9520, #15619, #9367, #9448, #11435 ) ) ;
#11313 = CARTESIAN_POINT ( 'NONE',  ( 5.611423337425062385, 41.22389019960463230, 93.92996380123798872 ) ) ;
#11314 = CARTESIAN_POINT ( 'NONE',  ( -2.416137431568557314, 39.07291177436112406, 91.11746380123798872 ) ) ;
#11315 = CARTESIAN_POINT ( 'NONE',  ( -4.211488180634966660, 48.16625856408043660, 80.45433879953087342 ) ) ;
#11316 = AXIS2_PLACEMENT_3D ( 'NONE', #3016, #10816, #9522 ) ;
#11317 = ADVANCED_FACE ( 'NONE', ( #6053 ), #10871, .F. ) ;
#11318 = CARTESIAN_POINT ( 'NONE',  ( -4.792503378000012582, 37.91763016944491227, 77.33669174070733732 ) ) ;
#11319 = ORIENTED_EDGE ( 'NONE', *, *, #1680, .F. ) ;
#11320 = CARTESIAN_POINT ( 'NONE',  ( 5.211422077973618450, 50.88905158406131335, 77.07967726685606635 ) ) ;
#11321 = VERTEX_POINT ( 'NONE', #3080 ) ;
#11322 = DIRECTION ( 'NONE',  ( -1.000000000000000000, -1.402518428993809243E-16, 6.308085367188358095E-15 ) ) ;
#11323 = LINE ( 'NONE', #12907, #18746 ) ;
#11324 = DIRECTION ( 'NONE',  ( 0.000000000000000000, 0.000000000000000000, 1.000000000000000000 ) ) ;
#11325 = ORIENTED_EDGE ( 'NONE', *, *, #20402, .F. ) ;
#11326 = EDGE_CURVE ( 'NONE', #26, #3490, #6206, .T. ) ;
#11327 = CARTESIAN_POINT ( 'NONE',  ( -7.677846259693481556, 40.96218137147969429, 93.55433879953098142 ) ) ;
#11328 = EDGE_CURVE ( 'NONE', #5035, #17146, #20723, .T. ) ;
#11329 = CARTESIAN_POINT ( 'NONE',  ( -4.859530362865108977, 37.19700002604054134, 79.54807357191100436 ) ) ;
#11330 = VECTOR ( 'NONE', #43, 1000.000000000000000 ) ;
#11331 = CARTESIAN_POINT ( 'NONE',  ( 5.214985644788185937, 40.92083184153662501, 92.55433879953100984 ) ) ;
#11332 = FACE_OUTER_BOUND ( 'NONE', #18567, .T. ) ;
#11333 = EDGE_CURVE ( 'NONE', #2806, #2513, #10806, .T. ) ;
#11334 = DIRECTION ( 'NONE',  ( 1.540237394707283727E-16, 1.793354297423763257E-16, -1.000000000000000000 ) ) ;
#11335 = ORIENTED_EDGE ( 'NONE', *, *, #20892, .T. ) ;
#11336 = FACE_OUTER_BOUND ( 'NONE', #18351, .T. ) ;
#11337 = DIRECTION ( 'NONE',  ( 0.3015081906286223301, -0.9534635866061452747, -1.245503830460468587E-16 ) ) ;
#11338 = ORIENTED_EDGE ( 'NONE', *, *, #10042, .F. ) ;
#11339 = FACE_OUTER_BOUND ( 'NONE', #11312, .T. ) ;
#11340 = LINE ( 'NONE', #3236, #16231 ) ;
#11341 = EDGE_CURVE ( 'NONE', #16624, #8340, #2967, .T. ) ;
#11342 = EDGE_CURVE ( 'NONE', #15997, #5268, #1489, .T. ) ;
#11343 = CARTESIAN_POINT ( 'NONE',  ( -5.782670150369643380, 50.47275727106970322, 76.07566230427023868 ) ) ;
#11344 = CARTESIAN_POINT ( 'NONE',  ( -1.187946976321873294, 48.86064447540922373, 95.29808879611699979 ) ) ;
#11345 = LINE ( 'NONE', #13240, #13715 ) ;
#11346 = DIRECTION ( 'NONE',  ( -1.000000000000000000, 0.000000000000000000, 0.000000000000000000 ) ) ;
#11347 = CARTESIAN_POINT ( 'NONE',  ( -1.183761187420877548, 49.81017696809242068, 92.55433879953098142 ) ) ;
#11348 = CARTESIAN_POINT ( 'NONE',  ( -0.8111795930268231869, 49.49551470481303284, 53.82100546619766845 ) ) ;
#11349 = EDGE_LOOP ( 'NONE', ( #16403, #18668, #6275, #5046 ) ) ;
#11350 = CARTESIAN_POINT ( 'NONE',  ( 1.937197196555007661, 52.84783582409303193, 77.09277561753447117 ) ) ;
#11351 = CARTESIAN_POINT ( 'NONE',  ( 0.5221537403065188432, 44.16218137147969003, 54.55433879953099563 ) ) ;
#11352 = ORIENTED_EDGE ( 'NONE', *, *, #8, .T. ) ;
#11353 = CARTESIAN_POINT ( 'NONE',  ( -7.783793320189392517, 41.25506035324961829, 78.45492795665607844 ) ) ;
#11354 = DIRECTION ( 'NONE',  ( 1.000000000000000000, -1.193617070626243484E-16, 0.000000000000000000 ) ) ;
#11355 = PLANE ( 'NONE',  #18413 ) ;
#11356 = ORIENTED_EDGE ( 'NONE', *, *, #6602, .F. ) ;
#11357 = CARTESIAN_POINT ( 'NONE',  ( 5.605612954821764582, 51.34764942893797013, 78.13212606300182017 ) ) ;
#11358 = CARTESIAN_POINT ( 'NONE',  ( -7.762578640187608237, 47.15103685007025547, 79.11815246340434271 ) ) ;
#11359 = ORIENTED_EDGE ( 'NONE', *, *, #20903, .T. ) ;
#11360 = DIRECTION ( 'NONE',  ( -0.3165065846431824870, -0.9485903129789529098, 0.000000000000000000 ) ) ;
#11361 = CARTESIAN_POINT ( 'NONE',  ( 8.378637954445377289, 41.81363803720061867, 78.41904468188381827 ) ) ;
#11362 = CARTESIAN_POINT ( 'NONE',  ( -0.2125050281363792815, 38.58189400963055959, 94.24246379953099506 ) ) ;
#11363 = ORIENTED_EDGE ( 'NONE', *, *, #17674, .T. ) ;
#11364 = FACE_OUTER_BOUND ( 'NONE', #16957, .T. ) ;
#11365 = SHAPE_REPRESENTATION ( 'MAS-160', ( #3756, #16674, #10231, #1051, #5447, #12932, #13611, #3743, #6463, #15663, #16337 ), #17367 ) ;
#11366 = CARTESIAN_POINT ( 'NONE',  ( 8.869748494521283888, 41.37692342661967615, 77.52492703482499792 ) ) ;
#11367 = CARTESIAN_POINT ( 'NONE',  ( 4.178421596892070156, 40.17206517740157778, 93.81371379953100131 ) ) ;
#11368 = VECTOR ( 'NONE', #16304, 1000.000000000000000 ) ;
#11369 = EDGE_LOOP ( 'NONE', ( #19188, #16166, #11930, #5226, #10141, #19430, #19695 ) ) ;
#11370 = DIRECTION ( 'NONE',  ( 0.9999689119394086223, -0.007885122365275665235, 1.526048693634353392E-16 ) ) ;
#11371 = PLANE ( 'NONE',  #245 ) ;
#11372 = CARTESIAN_POINT ( 'NONE',  ( -5.507377839757669591, 38.60475994759722340, 78.70824393732894464 ) ) ;
#11373 = ADVANCED_FACE ( 'NONE', ( #7974 ), #4241, .T. ) ;
#11374 = CARTESIAN_POINT ( 'NONE',  ( -5.754662135367683895, 50.49277077315122142, 75.98690818113186651 ) ) ;
#11375 = CARTESIAN_POINT ( 'NONE',  ( -4.532425740520046986, 37.70530639010522833, 76.20224062571769252 ) ) ;
#11376 = B_SPLINE_CURVE_WITH_KNOTS ( 'NONE', 3,
 ( #12354, #958, #15540, #20831, #15760, #20722, #7660, #1175, #14138, #9371, #4455, #2556 ),
 .UNSPECIFIED., .F., .F.,
 ( 4, 2, 2, 2, 2, 4 ),
 ( 0.000000000000000000, 7.773291567551462685E-05, 0.0001554658313510292537, 0.0003109316627020570437, 0.0004663974940530848609, 0.0006218633254041125696 ),
 .UNSPECIFIED. ) ;
#11377 = DIRECTION ( 'NONE',  ( 0.3165065846431826535, 0.9485903129789529098, 2.188653791613874008E-16 ) ) ;
#11378 = CARTESIAN_POINT ( 'NONE',  ( 4.432284427945813121, 36.14044538431356557, 77.43080938776617472 ) ) ;
#11379 = CARTESIAN_POINT ( 'NONE',  ( 8.436128353966983795, 40.07733635702963682, 79.00897045670630803 ) ) ;
#11380 = EDGE_LOOP ( 'NONE', ( #906, #20567, #16500, #19970 ) ) ;
#11381 = CARTESIAN_POINT ( 'NONE',  ( 0.5221537403065181771, 44.16218137147969003, 56.15433879953099705 ) ) ;
#11382 = PLANE ( 'NONE',  #18749 ) ;
#11383 = CARTESIAN_POINT ( 'NONE',  ( 0.5867509473165513079, 52.35421642379875351, 77.38375056423674891 ) ) ;
#11384 = CARTESIAN_POINT ( 'NONE',  ( 2.259191861956068692, 47.76843358786783966, 53.41730067788145675 ) ) ;
#11385 = ORIENTED_EDGE ( 'NONE', *, *, #5029, .F. ) ;
#11386 = EDGE_LOOP ( 'NONE', ( #1304, #12794, #16788, #15799 ) ) ;
#11387 = ADVANCED_BREP_SHAPE_REPRESENTATION ( '', ( #10973, #18366 ), #4082 ) ;
#11388 = FACE_OUTER_BOUND ( 'NONE', #5493, .T. ) ;
#11389 = CARTESIAN_POINT ( 'NONE',  ( 0.5221537403065064087, 48.16218137147969003, 61.55433879953100273 ) ) ;
#11390 = DIRECTION ( 'NONE',  ( 1.000000000000000000, 0.000000000000000000, 0.000000000000000000 ) ) ;
#11391 = DIRECTION ( 'NONE',  ( -1.000000000000000000, -5.084437235940625660E-16, -0.000000000000000000 ) ) ;
#11392 = CARTESIAN_POINT ( 'NONE',  ( -4.622577041588897373, 46.56120873422322859, 94.90746379782396502 ) ) ;
#11393 = CARTESIAN_POINT ( 'NONE',  ( 10.77494014480653917, 42.96218137147968008, 61.80715055817104542 ) ) ;
#11394 = DIRECTION ( 'NONE',  ( 0.3165065846431826535, 0.9485903129789529098, 2.188653791613874008E-16 ) ) ;
#11395 = CARTESIAN_POINT ( 'NONE',  ( -3.860974883312077832, 38.44857360937989199, 79.54845644658969661 ) ) ;
#11396 = CARTESIAN_POINT ( 'NONE',  ( 29.63948732994508006, 43.16218137147969003, 76.90433879953101837 ) ) ;
#11397 = CARTESIAN_POINT ( 'NONE',  ( -2.416137431568557314, 39.07291177436112406, 91.11746380123798872 ) ) ;
#11398 = ORIENTED_EDGE ( 'NONE', *, *, #20230, .F. ) ;
#11399 = CARTESIAN_POINT ( 'NONE',  ( 2.522153740306505298, 50.16218137147969713, 85.15433879953098995 ) ) ;
#11400 = ADVANCED_FACE ( 'NONE', ( #13080 ), #6466, .T. ) ;
#11401 = VERTEX_POINT ( 'NONE', #14460 ) ;
#11402 = DIRECTION ( 'NONE',  ( 0.007885122365275663500, 0.9999689119394085113, 1.805443505845543142E-16 ) ) ;
#11403 = CARTESIAN_POINT ( 'NONE',  ( 5.242046259730475555, 50.86759873786404285, 78.66925348396956963 ) ) ;
#11404 = CARTESIAN_POINT ( 'NONE',  ( 8.907015937602837496, 41.48861631773759484, 77.50814924735175282 ) ) ;
#11405 = CARTESIAN_POINT ( 'NONE',  ( 9.333517871656532350, 42.76686967087471913, 77.60952670463396430 ) ) ;
#11406 = VERTEX_POINT ( 'NONE', #11389 ) ;
#11407 = CARTESIAN_POINT ( 'NONE',  ( 6.268485860042931179, 37.45252770006494103, 75.44618574453703275 ) ) ;
#11408 = CARTESIAN_POINT ( 'NONE',  ( 0.4030602640235012579, 52.96930499935337622, 79.54130260543404063 ) ) ;
#11409 = CARTESIAN_POINT ( 'NONE',  ( 8.095534471974675128, 41.01620876067410393, 79.49089192870339105 ) ) ;
#11410 = CARTESIAN_POINT ( 'NONE',  ( 4.178324861372344934, 51.50200996931119590, 75.94208404623037723 ) ) ;
#11411 = FACE_OUTER_BOUND ( 'NONE', #3854, .T. ) ;
#11412 = ORIENTED_EDGE ( 'NONE', *, *, #18213, .F. ) ;
#11413 = CARTESIAN_POINT ( 'NONE',  ( 0.3201111382462865640, 51.36399839264385037, 78.50066232894263862 ) ) ;
#11414 = ORIENTED_EDGE ( 'NONE', *, *, #14856, .T. ) ;
#11415 = CARTESIAN_POINT ( 'NONE',  ( 6.828503391016846891, 43.33193468930419101, 92.75808880123800293 ) ) ;
#11416 = FACE_OUTER_BOUND ( 'NONE', #16309, .T. ) ;
#11417 = CARTESIAN_POINT ( 'NONE',  ( -3.532917577324402369, 36.21708460058427193, 78.46683879953087626 ) ) ;
#11418 = PLANE ( 'NONE',  #10633 ) ;
#11419 = EDGE_CURVE ( 'NONE', #13402, #585, #10004, .T. ) ;
#11420 = PRODUCT_DEFINITION_SHAPE ( 'NONE', 'NONE',  #21044 ) ;
#11421 = CARTESIAN_POINT ( 'NONE',  ( 5.622879012935364962, 37.74899935393362682, 78.37107466246847309 ) ) ;
#11422 = ORIENTED_EDGE ( 'NONE', *, *, #11204, .T. ) ;
#11423 = CARTESIAN_POINT ( 'NONE',  ( -4.519095118814111522, 36.94553422482819371, 76.36459416792565946 ) ) ;
#11424 = ORIENTED_EDGE ( 'NONE', *, *, #9892, .F. ) ;
#11425 = CARTESIAN_POINT ( 'NONE',  ( -7.723582874747324745, 47.23591325229828186, 77.58227997600145898 ) ) ;
#11426 = DIRECTION ( 'NONE',  ( -1.402518428993831183E-16, 1.000000000000000000, -3.469446951953617640E-16 ) ) ;
#11427 = CARTESIAN_POINT ( 'NONE',  ( -0.9988176903691428077, 49.83852402762217082, 94.39871380123798872 ) ) ;
#11428 = ORIENTED_EDGE ( 'NONE', *, *, #16653, .F. ) ;
#11429 = CARTESIAN_POINT ( 'NONE',  ( 1.979752811602338181, 52.23166353794246675, 77.14917161731061412 ) ) ;
#11430 = CARTESIAN_POINT ( 'NONE',  ( -5.945795452124602143, 37.96218137147967298, 45.55433879953098852 ) ) ;
#11431 = CARTESIAN_POINT ( 'NONE',  ( 5.913630530257057316, 51.12012925366870064, 76.09715583564816654 ) ) ;
#11432 = ADVANCED_FACE ( 'NONE', ( #1903 ), #14873, .F. ) ;
#11433 = CARTESIAN_POINT ( 'NONE',  ( -3.349688636638950889, 52.21127678364309332, 78.10580938776615767 ) ) ;
#11434 = LINE ( 'NONE', #12709, #9274 ) ;
#11435 = ORIENTED_EDGE ( 'NONE', *, *, #20141, .F. ) ;
#11436 = CARTESIAN_POINT ( 'NONE',  ( -4.448383556050954368, 51.42618962001968441, 76.01002907825849775 ) ) ;
#11437 = LINE ( 'NONE', #17909, #4189 ) ;
#11438 = VERTEX_POINT ( 'NONE', #8289 ) ;
#11439 = CARTESIAN_POINT ( 'NONE',  ( -2.677692965280757953, 48.66802378075904301, 95.05433879953109511 ) ) ;
#11440 = CARTESIAN_POINT ( 'NONE',  ( -7.555311451759470387, 40.50225460051125026, 77.45762758118813451 ) ) ;
#11441 = CARTESIAN_POINT ( 'NONE',  ( -4.355629557941309571, 50.57269264884984494, 75.36324311589748959 ) ) ;
#11442 = CARTESIAN_POINT ( 'NONE',  ( -4.884656273474449861, 44.39824779480852612, 91.78246379611699979 ) ) ;
#11443 = CARTESIAN_POINT ( 'NONE',  ( -4.622577041588896485, 46.56120873422322859, 92.40746379782397923 ) ) ;
#11444 = ADVANCED_FACE ( 'NONE', ( #8073 ), #4758, .T. ) ;
#11446 = EDGE_CURVE ( 'NONE', #15205, #15934, #19341, .T. ) ;
#11445 = DIRECTION ( 'NONE',  ( 0.000000000000000000, -1.000000000000000000, 0.000000000000000000 ) ) ;
#11447 = LINE ( 'NONE', #11347, #749 ) ;
#11448 = EDGE_CURVE ( 'NONE', #3959, #14425, #6697, .T. ) ;
#11449 = VECTOR ( 'NONE', #4866, 1000.000000000000000 ) ;
#11450 = CARTESIAN_POINT ( 'NONE',  ( 5.468950880928916014, 50.69396025583560572, 75.98827401121828018 ) ) ;
#11451 = ORIENTED_EDGE ( 'NONE', *, *, #5810, .F. ) ;
#11452 = CARTESIAN_POINT ( 'NONE',  ( 0.5221537403065048544, 44.16218137147969713, 82.55433879953099563 ) ) ;
#11453 = VERTEX_POINT ( 'NONE', #12861 ) ;
#11454 = CARTESIAN_POINT ( 'NONE',  ( -7.919272757704022503, 41.67135357887591596, 77.69952636542143409 ) ) ;
#11455 = EDGE_CURVE ( 'NONE', #19954, #16819, #14771, .T. ) ;
#11456 = FACE_BOUND ( 'NONE', #9018, .T. ) ;
#11457 = LINE ( 'NONE', #19205, #19101 ) ;
#11458 = ORIENTED_EDGE ( 'NONE', *, *, #487, .T. ) ;
#11459 = B_SPLINE_CURVE_WITH_KNOTS ( 'NONE', 3,
 ( #1230, #7515, #912, #18995, #7401, #4307, #4208, #6114, #13890, #10733, #20375, #9117, #2618, #15606, #5919, #12416, #18895, #10832, #17296 ),
 .UNSPECIFIED., .F., .F.,
 ( 4, 1, 1, 1, 1, 1, 1, 1, 1, 1, 1, 1, 1, 1, 1, 1, 4 ),
 ( 0.000000000000000000, 0.1068357064626556524, 0.2062857352809531475, 0.2975635024103033266, 0.3806658168942347320, 0.4556695234475648948, 0.5225582867794639208, 0.5822950421180911329, 0.6340416422721021350, 0.6795378779249960921, 0.7218021178892558565, 0.7627433693661896941, 0.8042009657065650741, 0.8472253578321278233, 0.8932235139329930407, 0.9440217631200717996, 0.9999999999999998890 ),
 .UNSPECIFIED. ) ;
#11460 = PLANE ( 'NONE',  #3735 ) ;
#11461 = CARTESIAN_POINT ( 'NONE',  ( -4.756616962678589466, 37.12098204292738757, 75.36046818803191627 ) ) ;
#11462 = MANIFOLD_SOLID_BREP ( 'Stock-MAS-160-1', #7469 ) ;
#11463 = ORIENTED_EDGE ( 'NONE', *, *, #15889, .F. ) ;
#11464 = DIRECTION ( 'NONE',  ( 1.540237394707284220E-16, 1.793354297423764243E-16, -1.000000000000000000 ) ) ;
#11465 = LINE ( 'NONE', #11568, #7457 ) ;
#11466 = CARTESIAN_POINT ( 'NONE',  ( 3.948530577815480225, 39.69684013992245752, 93.14871379953099506 ) ) ;
#11467 = VERTEX_POINT ( 'NONE', #6574 ) ;
#11468 = FACE_OUTER_BOUND ( 'NONE', #15513, .T. ) ;
#11469 = CARTESIAN_POINT ( 'NONE',  ( -4.238691248938474487, 37.51317230028318050, 77.97288938838477179 ) ) ;
#11470 = ORIENTED_EDGE ( 'NONE', *, *, #4537, .F. ) ;
#11471 = CARTESIAN_POINT ( 'NONE',  ( 5.520808673089612206, 50.66245348763631284, 78.85200372869584839 ) ) ;
#11472 = CARTESIAN_POINT ( 'NONE',  ( 1.925877929012052903, 52.84973764076755032, 75.80025412519856332 ) ) ;
#11473 = DIRECTION ( 'NONE',  ( 0.000000000000000000, 0.000000000000000000, 1.000000000000000000 ) ) ;
#11474 = CARTESIAN_POINT ( 'NONE',  ( 6.375754489315274220, 49.85394395361436892, 75.81347835631012799 ) ) ;
#11475 = CARTESIAN_POINT ( 'NONE',  ( 0.9565776152847129676, 52.96313783584191270, 76.77464780632124075 ) ) ;
#11476 = ADVANCED_FACE ( 'NONE', ( #8392 ), #7487, .T. ) ;
#11477 = CARTESIAN_POINT ( 'NONE',  ( 4.766132218518882802, 37.29877637478772812, 75.41205140984322952 ) ) ;
#11478 = B_SPLINE_CURVE_WITH_KNOTS ( 'NONE', 3,
 ( #7999, #14591, #119, #9927, #12888, #5210, #8419, #216, #18200, #19790, #3620, #1730, #17, #6492, #13001 ),
 .UNSPECIFIED., .F., .F.,
 ( 4, 1, 1, 1, 1, 1, 1, 1, 1, 1, 1, 1, 4 ),
 ( 0.000000000000000000, 0.1142047618744220089, 0.2098279651953024738, 0.2930641324527410441, 0.3714084400245239448, 0.4142179382887971051, 0.4671782061414135323, 0.5290873093409070860, 0.6015893617863945497, 0.6852532414128420513, 0.7789222961280750646, 0.8837899115430479791, 1.000000000000000000 ),
 .UNSPECIFIED. ) ;
#11479 = CARTESIAN_POINT ( 'NONE',  ( 7.675798357370772429, 40.16299717330817742, 77.69330938776616335 ) ) ;
#11480 = AXIS2_PLACEMENT_3D ( 'NONE', #11284, #16481, #14666 ) ;
#11481 = ORIENTED_EDGE ( 'NONE', *, *, #14396, .F. ) ;
#11482 = CARTESIAN_POINT ( 'NONE',  ( -4.244920859621176490, 37.49018728506336373, 76.00056232034928883 ) ) ;
#11483 = CARTESIAN_POINT ( 'NONE',  ( 9.353328126263708242, 42.82624226067153472, 76.54645538997905874 ) ) ;
#11484 = EDGE_CURVE ( 'NONE', #2608, #559, #5389, .T. ) ;
#11485 = CARTESIAN_POINT ( 'NONE',  ( 0.5221537403065014127, 44.16218137147968292, 76.16022115247204738 ) ) ;
#11486 = CARTESIAN_POINT ( 'NONE',  ( 2.002611129390325484, 52.83679921599847518, 78.99455554248785916 ) ) ;
#11487 =( BOUNDED_CURVE ( )  B_SPLINE_CURVE ( 2, ( #2713, #17496, #15704, #12609, #1125, #19095, #12917, #12502, #9324, #2920, #2820 ),
 .UNSPECIFIED., .F., .T. ) 
 B_SPLINE_CURVE_WITH_KNOTS ( ( 3, 2, 2, 2, 2, 3 ),
 ( 0.5333811345117427383, 0.5500000000000000444, 0.5749999999999999556, 0.5999999999999999778, 0.6250000000000000000, 0.6333811345117427161 ),
 .UNSPECIFIED. ) 
 CURVE ( )  GEOMETRIC_REPRESENTATION_ITEM ( )  RATIONAL_B_SPLINE_CURVE ( ( 0.9660722070828660080, 0.9493985675960723292, 1.000000000000000000, 0.9238795325112867385, 1.000000000000000000, 0.9238795325112867385, 1.000000000000000000, 0.9238795325112867385, 1.000000000000000000, 0.9744809649152141873, 0.9660722070828660080 ) ) 
 REPRESENTATION_ITEM ( '' )  );
#11488 = ADVANCED_FACE ( 'NONE', ( #19959 ), #3804, .F. ) ;
#11489 = VERTEX_POINT ( 'NONE', #13592 ) ;
#11490 = FACE_OUTER_BOUND ( 'NONE', #13727, .T. ) ;
#11491 = ORIENTED_EDGE ( 'NONE', *, *, #9785, .T. ) ;
#11492 = AXIS2_PLACEMENT_3D ( 'NONE', #11393, #6577, #17647 ) ;
#11493 = CARTESIAN_POINT ( 'NONE',  ( 5.544968037009670780, 45.50804040601273925, 93.69558880294498238 ) ) ;
#11494 = CARTESIAN_POINT ( 'NONE',  ( 0.5221537403065191763, 44.16218137147969003, 53.55433879953099563 ) ) ;
#11495 = CARTESIAN_POINT ( 'NONE',  ( 8.328612408207245466, 41.65204230202461133, 77.51978620826790234 ) ) ;
#11496 = CARTESIAN_POINT ( 'NONE',  ( -3.981178359372548492, 46.76218137147973408, 94.16433880294496817 ) ) ;
#11497 = CARTESIAN_POINT ( 'NONE',  ( -5.510796958474739604, 38.60848837797752964, 76.73301527011911105 ) ) ;
#11498 = VECTOR ( 'NONE', #718, 1000.000000000000000 ) ;
#11499 = CARTESIAN_POINT ( 'NONE',  ( 6.238653020734597376, 49.95521528567088154, 77.60602934391619101 ) ) ;
#11500 = DIRECTION ( 'NONE',  ( 5.626130192357176673E-16, 1.831515347669941892E-30, -1.000000000000000000 ) ) ;
#11501 = DIRECTION ( 'NONE',  ( -1.540237394707284220E-16, -1.793354297423764243E-16, 1.000000000000000000 ) ) ;
#11502 = CARTESIAN_POINT ( 'NONE',  ( 1.352400422481993658, 50.46853102219002096, 94.32058880123798872 ) ) ;
#11503 = VERTEX_POINT ( 'NONE', #11908 ) ;
#11504 = DIRECTION ( 'NONE',  ( -1.540237394707284467E-16, -1.793354297423764243E-16, 1.000000000000000000 ) ) ;
#11505 = VECTOR ( 'NONE', #199, 1000.000000000000000 ) ;
#11506 = CARTESIAN_POINT ( 'NONE',  ( -5.827090762987216621, 50.44101592763561115, 78.49957729094111869 ) ) ;
#11507 = EDGE_CURVE ( 'NONE', #6991, #264, #1389, .T. ) ;
#11508 = FACE_OUTER_BOUND ( 'NONE', #4268, .T. ) ;
#11509 = CARTESIAN_POINT ( 'NONE',  ( 2.522153740306504854, 49.81903562097208038, 85.15433879953098995 ) ) ;
#11510 = LINE ( 'NONE', #14787, #13902 ) ;
#11511 = ORIENTED_EDGE ( 'NONE', *, *, #11701, .F. ) ;
#11512 = CARTESIAN_POINT ( 'NONE',  ( 6.837774032321189743, 37.85932018500469809, 76.05683950549904182 ) ) ;
#11513 = CARTESIAN_POINT ( 'NONE',  ( 7.680900363438858847, 40.16312786850421190, 78.17527862778651127 ) ) ;
#11514 = DIRECTION ( 'NONE',  ( -0.7071067811865434649, 0.7071067811865515695, 0.000000000000000000 ) ) ;
#11515 = CARTESIAN_POINT ( 'NONE',  ( 0.3123767374396226315, 49.66473798958180197, 92.45433879953097289 ) ) ;
#11516 = EDGE_LOOP ( 'NONE', ( #20916, #3098, #16762, #18726 ) ) ;
#11517 = LINE ( 'NONE', #11413, #12821 ) ;
#11518 = CIRCLE ( 'NONE', #10165, 8.799999999999997158 ) ;
#11519 = ORIENTED_EDGE ( 'NONE', *, *, #20241, .T. ) ;
#11520 = CARTESIAN_POINT ( 'NONE',  ( 4.987494971863720927, 47.58855820898865829, 95.02371380294496817 ) ) ;
#11521 = CARTESIAN_POINT ( 'NONE',  ( 0.4682140828567994961, 52.36204277483403757, 75.98649299885811104 ) ) ;
#11522 = CARTESIAN_POINT ( 'NONE',  ( -3.533008836142939035, 36.21715200979739535, 78.43912781517941823 ) ) ;
#11523 = EDGE_CURVE ( 'NONE', #5069, #18148, #17578, .T. ) ;
#11524 = DIRECTION ( 'NONE',  ( 0.5800177190770223756, 0.8146038580541393737, 2.354238310054622780E-16 ) ) ;
#11525 = ORIENTED_EDGE ( 'NONE', *, *, #13907, .F. ) ;
#11526 = DIRECTION ( 'NONE',  ( 1.000000000000000000, 0.000000000000000000, 0.000000000000000000 ) ) ;
#11527 = VECTOR ( 'NONE', #9341, 1000.000000000000000 ) ;
#11528 = ORIENTED_EDGE ( 'NONE', *, *, #20137, .T. ) ;
#11529 = DIRECTION ( 'NONE',  ( -5.626130192357176673E-16, -1.831515347669941892E-30, 1.000000000000000000 ) ) ;
#11530 = CARTESIAN_POINT ( 'NONE',  ( 3.873544841512769121, 48.16470079461351617, 94.75578198602110547 ) ) ;
#11531 = CARTESIAN_POINT ( 'NONE',  ( -0.9988176903691428077, 49.83852402762217082, 95.64871380123798872 ) ) ;
#11532 = ORIENTED_EDGE ( 'NONE', *, *, #10851, .T. ) ;
#11533 = CARTESIAN_POINT ( 'NONE',  ( 8.244331251587055931, 41.40382638133797144, 77.92171669569661674 ) ) ;
#11534 = CARTESIAN_POINT ( 'NONE',  ( -5.889261015154378498, 37.95762057880577345, 79.03330530165142420 ) ) ;
#11535 = CARTESIAN_POINT ( 'NONE',  ( 4.819906901611561878, 40.37133391887874012, 92.55433879953100984 ) ) ;
#11536 = CARTESIAN_POINT ( 'NONE',  ( 2.522153740306507519, 49.81903562097208038, 69.15433879953098995 ) ) ;
#11537 = DIRECTION ( 'NONE',  ( 1.000000000000000000, 0.000000000000000000, 0.000000000000000000 ) ) ;
#11538 = ORIENTED_EDGE ( 'NONE', *, *, #1121, .F. ) ;
#11539 = PLANE ( 'NONE',  #4076 ) ;
#11540 = EDGE_CURVE ( 'NONE', #9657, #3218, #15386, .T. ) ;
#11541 = CARTESIAN_POINT ( 'NONE',  ( 1.083001295814570053, 52.34297901104275041, 76.77198585835439815 ) ) ;
#11542 = ORIENTED_EDGE ( 'NONE', *, *, #18306, .T. ) ;
#11543 = CARTESIAN_POINT ( 'NONE',  ( 4.588242150565980282, 52.09914025984591746, 78.23954818826248925 ) ) ;
#11544 = DIRECTION ( 'NONE',  ( -0.7071067811865506814, 0.7071067811865443531, -2.453269466693389746E-16 ) ) ;
#11545 = VECTOR ( 'NONE', #17437, 1000.000000000000000 ) ;
#11546 = DIRECTION ( 'NONE',  ( 1.000000000000000000, 0.000000000000000000, 0.000000000000000000 ) ) ;
#11547 = CARTESIAN_POINT ( 'NONE',  ( 3.722706642241001784, 40.32076742321550000, 95.99159722619801016 ) ) ;
#11548 = ADVANCED_FACE ( 'NONE', ( #20072 ), #16895, .F. ) ;
#11549 = CARTESIAN_POINT ( 'NONE',  ( -4.812088799398940075, 42.22067586467031930, 93.81371379782397923 ) ) ;
#11550 = CARTESIAN_POINT ( 'NONE',  ( 5.835344820533724608, 37.14302097153727544, 76.09175310361966638 ) ) ;
#11551 = DIRECTION ( 'NONE',  ( 0.000000000000000000, 1.000000000000000000, 0.000000000000000000 ) ) ;
#11552 = CARTESIAN_POINT ( 'NONE',  ( 5.552985721865087321, 50.63188710396593706, 76.09715583564816654 ) ) ;
#11554 = EDGE_CURVE ( 'NONE', #5907, #8246, #722, .T. ) ;
#11553 = AXIS2_PLACEMENT_3D ( 'NONE', #13445, #19917, #5341 ) ;
#11555 = ORIENTED_EDGE ( 'NONE', *, *, #324, .F. ) ;
#11556 = DIRECTION ( 'NONE',  ( 0.5000000000000061062, 1.204669080539463149E-16, 0.8660254037844351549 ) ) ;
#11557 = FACE_OUTER_BOUND ( 'NONE', #12100, .T. ) ;
#11558 = VECTOR ( 'NONE', #6314, 1000.000000000000000 ) ;
#11559 = ORIENTED_EDGE ( 'NONE', *, *, #19670, .F. ) ;
#11560 = DIRECTION ( 'NONE',  ( 0.9539696396349525154, -0.2999031954727372495, 9.315070279690337353E-17 ) ) ;
#11561 = CARTESIAN_POINT ( 'NONE',  ( 9.350990972312333227, 42.81923766201297354, 78.59572304307680213 ) ) ;
#11562 = AXIS2_PLACEMENT_3D ( 'NONE', #6659, #19840, #2089 ) ;
#11563 = EDGE_LOOP ( 'NONE', ( #19354, #13642, #11809, #15874, #11126, #1628, #717, #6155, #5257, #12124, #1512, #20213 ) ) ;
#11564 = VECTOR ( 'NONE', #11638, 1000.000000000000114 ) ;
#11565 = CARTESIAN_POINT ( 'NONE',  ( -5.728661668566968679, 37.83899231081794312, 75.70067668752250256 ) ) ;
#11566 = ORIENTED_EDGE ( 'NONE', *, *, #11714, .T. ) ;
#11567 = DIRECTION ( 'NONE',  ( 0.7071067811865433539, 0.7071067811865516806, -0.000000000000000000 ) ) ;
#11568 = CARTESIAN_POINT ( 'NONE',  ( -1.477846259693499809, 47.62628298661744708, 45.55433879953100273 ) ) ;
#11569 = CARTESIAN_POINT ( 'NONE',  ( 4.987494971863720927, 47.58855820898865829, 94.71121379953099506 ) ) ;
#11570 = EDGE_LOOP ( 'NONE', ( #3291, #14282, #18057, #20406 ) ) ;
#11571 = CARTESIAN_POINT ( 'NONE',  ( 0.6135278437555422570, 52.96173443653181323, 77.38466869867853859 ) ) ;
#11572 = CARTESIAN_POINT ( 'NONE',  ( -4.428896237227788468, 37.65366906320820561, 77.91201545794896788 ) ) ;
#11573 = CARTESIAN_POINT ( 'NONE',  ( -1.187946976321872850, 48.86064447540922373, 94.36058879953097289 ) ) ;
#11574 = VECTOR ( 'NONE', #8979, 1000.000000000000000 ) ;
#11575 = ORIENTED_EDGE ( 'NONE', *, *, #8959, .F. ) ;
#11576 = CARTESIAN_POINT ( 'NONE',  ( -4.798777446476682584, 51.17581097466058537, 76.24916814194597237 ) ) ;
#11577 = CARTESIAN_POINT ( 'NONE',  ( 30.43948732994507722, 43.16218137147969003, 74.70433879953098710 ) ) ;
#11578 = LINE ( 'NONE', #18052, #2379 ) ;
#11579 =( NAMED_UNIT ( * ) SI_UNIT ( $, .STERADIAN. ) SOLID_ANGLE_UNIT ( ) );
#11580 = CIRCLE ( 'NONE', #1734, 6.199999999999999289 ) ;
#11581 = CARTESIAN_POINT ( 'NONE',  ( -4.530198942227657177, 37.70355750481248691, 76.15642697799287930 ) ) ;
#11582 = VECTOR ( 'NONE', #973, 1000.000000000000000 ) ;
#11583 = CARTESIAN_POINT ( 'NONE',  ( -7.677846259693485109, 51.36218137147968577, 80.55433879953099563 ) ) ;
#11584 = ORIENTED_EDGE ( 'NONE', *, *, #20785, .F. ) ;
#11585 = CARTESIAN_POINT ( 'NONE',  ( 4.600886763243814848, 37.18069802247041622, 75.46362501775257670 ) ) ;
#11586 = VECTOR ( 'NONE', #19361, 1000.000000000000227 ) ;
#11587 = ORIENTED_EDGE ( 'NONE', *, *, #8291, .T. ) ;
#11588 = DIRECTION ( 'NONE',  ( 0.3165065846431828200, 0.9485903129789527988, 0.000000000000000000 ) ) ;
#11589 = DIRECTION ( 'NONE',  ( 1.000000000000000000, 0.000000000000000000, -0.000000000000000000 ) ) ;
#11590 = CYLINDRICAL_SURFACE ( 'NONE', #7572, 6.200000000000000178 ) ;
#11591 = CARTESIAN_POINT ( 'NONE',  ( 2.118765075475726345, 52.81613201993158668, 78.36533242353944217 ) ) ;
#11592 = ORIENTED_EDGE ( 'NONE', *, *, #11045, .T. ) ;
#11593 = EDGE_LOOP ( 'NONE', ( #19174, #15090, #16838, #14205 ) ) ;
#11594 = PLANE ( 'NONE',  #6558 ) ;
#11595 = ORIENTED_EDGE ( 'NONE', *, *, #20911, .T. ) ;
#11596 = EDGE_CURVE ( 'NONE', #19492, #16873, #12218, .T. ) ;
#11597 = B_SPLINE_CURVE_WITH_KNOTS ( 'NONE', 3,
 ( #5712, #18812, #6141, #18912, #9353, #12531, #13912, #14224, #4324, #7532, #15838, #11054, #1250, #1155, #17321, #7742 ),
 .UNSPECIFIED., .F., .F.,
 ( 4, 2, 2, 2, 2, 2, 2, 4 ),
 ( 0.000000000000000000, 0.0005762146036707721389, 0.0008643219055061592384, 0.001152429207341546229, 0.001440536509176933329, 0.001728643811012320428, 0.002016751112847707528, 0.002304858414683094627 ),
 .UNSPECIFIED. ) ;
#11598 = CARTESIAN_POINT ( 'NONE',  ( 7.680445814051256370, 40.16232446084477914, 76.89670332066808101 ) ) ;
#11600 = ADVANCED_FACE ( 'NONE', ( #4115 ), #13913, .F. ) ;
#11599 = CARTESIAN_POINT ( 'NONE',  ( 4.461908506452709311, 51.26762488673620055, 77.64500276804245971 ) ) ;
#11601 = CARTESIAN_POINT ( 'NONE',  ( -0.9143671159618040889, 52.84414119167043822, 76.25586683505548535 ) ) ;
#11602 = CARTESIAN_POINT ( 'NONE',  ( 19.23948732994504240, 27.61837231449496599, 84.70433879953101552 ) ) ;
#11603 = B_SPLINE_SURFACE_WITH_KNOTS ( 'NONE', 3, 1, ( 
 ( #716, #7198 ),
 ( #823, #15089 ),
 ( #2206, #12014 ),
 ( #13700, #10209 ),
 ( #8706, #10317 ),
 ( #3798, #11794 ),
 ( #18269, #16791 ),
 ( #15189, #20175 ),
 ( #5605, #3688 ),
 ( #10639, #20274 ),
 ( #4004, #15512 ),
 ( #2423, #13798 ),
 ( #6884, #5704 ),
 ( #17106, #9447 ),
 ( #14217, #4531 ),
 ( #20694, #1039 ),
 ( #10945, #15933 ),
 ( #10845, #12524 ),
 ( #4318, #4628 ) ),
 .UNSPECIFIED., .F., .F., .F.,
 ( 4, 1, 1, 1, 1, 1, 1, 1, 1, 1, 1, 1, 1, 1, 1, 1, 4 ),
 ( 2, 2 ),
 ( 0.000000000000000000, 0.06302581646095750667, 0.1222495429959427476, 0.1789669701231155763, 0.2332877456213924006, 0.2860909212508800925, 0.3384954837963008445, 0.3911857795644178570, 0.4453574251251987137, 0.5015394511440722791, 0.5602660668541803446, 0.6223358252984214634, 0.6886061413240012197, 0.7590929558684775813, 0.8342439359547982880, 0.9143471077142913961, 1.000000000000000000 ),
 ( 0.000000000000000000, 1.000000000000000000 ),
 .UNSPECIFIED. ) ;
#11604 = CARTESIAN_POINT ( 'NONE',  ( 5.239313537742215310, 50.86510457629285042, 78.30875056423674607 ) ) ;
#11605 = CARTESIAN_POINT ( 'NONE',  ( 31.07218010054375412, 45.56218137147968861, 70.80574467885102763 ) ) ;
#11606 = CARTESIAN_POINT ( 'NONE',  ( -3.054046897975729813, 36.78819506682361151, 76.51650556680409920 ) ) ;
#11607 = CARTESIAN_POINT ( 'NONE',  ( -4.533682039091601723, 37.71094493724306318, 76.26481528174605273 ) ) ;
#11608 = EDGE_CURVE ( 'NONE', #15667, #3488, #10854, .T. ) ;
#11609 = CARTESIAN_POINT ( 'NONE',  ( -2.416137431568557314, 39.07291177436112406, 92.36746380123797451 ) ) ;
#11610 = VECTOR ( 'NONE', #6260, 1000.000000000000000 ) ;
#11611 = ORIENTED_EDGE ( 'NONE', *, *, #2074, .T. ) ;
#11612 = CARTESIAN_POINT ( 'NONE',  ( 0.4858785009097955077, 52.96635066793365354, 75.98243536310876323 ) ) ;
#11613 = AXIS2_PLACEMENT_3D ( 'NONE', #7571, #14053, #2782 ) ;
#11614 =( BOUNDED_CURVE ( )  B_SPLINE_CURVE ( 2, ( #19244, #12864, #19344, #14989, #14875, #15098, #5084, #195, #12974, #18078, #97, #3497, #8395, #16484, #19454, #296, #6893, #9904, #406, #13397, #1812, #13083, #1703, #6469, #4869, #18180, #10007, #6788, #13185, #19659, #16587, #3596, #11392, #6576, #10104 ),
 .UNSPECIFIED., .F., .T. ) 
 B_SPLINE_CURVE_WITH_KNOTS ( ( 3, 2, 2, 2, 2, 2, 2, 2, 2, 2, 2, 2, 2, 2, 2, 2, 2, 3 ),
 ( 0.3500748721534128194, 0.3736316088721369777, 0.4075981187696039454, 0.4415646286670709131, 0.4755311385645378808, 0.5094976484620048485, 0.5434641583594719272, 0.5774306682569388949, 0.6113971781544058626, 0.6453636880518728303, 0.6793301979493397980, 0.7132967078468067657, 0.7472632177442737333, 0.7812297276417408121, 0.8151962375392077798, 0.8491627474366747474, 0.8831292573341417151, 0.9149214517709542971 ),
 .UNSPECIFIED. ) 
 CURVE ( )  GEOMETRIC_REPRESENTATION_ITEM ( )  RATIONAL_B_SPLINE_CURVE ( ( 0.9676416783622849849, 0.9472082996766311158, 1.000000000000000000, 0.9238795325112867385, 1.000000000000000000, 0.9238795325112867385, 1.000000000000000000, 0.9238795325112867385, 1.000000000000000000, 0.9238795325112867385, 1.000000000000000000, 0.9238795325112867385, 1.000000000000000000, 0.9238795325112867385, 1.000000000000000000, 0.9238795325112867385, 1.000000000000000000, 0.9238795325112867385, 1.000000000000000000, 0.9238795325112867385, 1.000000000000000000, 0.9238795325112867385, 1.000000000000000000, 0.9238795325112867385, 1.000000000000000000, 0.9238795325112867385, 1.000000000000000000, 0.9238795325112867385, 1.000000000000000000, 0.9238795325112867385, 1.000000000000000000, 0.9238795325112867385, 1.000000000000000000, 0.9287522706828729158, 0.9908783657868658334 ) ) 
 REPRESENTATION_ITEM ( '' )  );
#11615 = CARTESIAN_POINT ( 'NONE',  ( 2.035123479059382401, 36.10296785094196537, 72.45433879953085921 ) ) ;
#11616 = CARTESIAN_POINT ( 'NONE',  ( -4.893796645199854467, 37.22231114847117084, 78.64904841171450300 ) ) ;
#11617 = CARTESIAN_POINT ( 'NONE',  ( -7.079975527142585712, 43.92211762787398044, 72.45432679953087529 ) ) ;
#11618 = CARTESIAN_POINT ( 'NONE',  ( 9.178784097065811665, 42.30312273229867515, 78.05372954401303787 ) ) ;
#11619 = ORIENTED_EDGE ( 'NONE', *, *, #8726, .T. ) ;
#11620 = VECTOR ( 'NONE', #9783, 1000.000000000000000 ) ;
#11621 = CARTESIAN_POINT ( 'NONE',  ( 0.6035869791250174643, 52.96772377251001984, 79.54835876252475657 ) ) ;
#11622 = CARTESIAN_POINT ( 'NONE',  ( 6.604417847172709521, 37.69257239881283539, 78.19824744938543404 ) ) ;
#11623 = CARTESIAN_POINT ( 'NONE',  ( 4.214696258237026427, 51.48399209946829558, 75.85240097884792476 ) ) ;
#11624 = FACE_OUTER_BOUND ( 'NONE', #3009, .T. ) ;
#11625 = ORIENTED_EDGE ( 'NONE', *, *, #8459, .T. ) ;
#11626 = CARTESIAN_POINT ( 'NONE',  ( 8.951667845840693971, 41.62244091939069790, 76.38301527011910252 ) ) ;
#11627 = CARTESIAN_POINT ( 'NONE',  ( -3.349688636638950889, 52.21127678364309332, 76.69845644658968808 ) ) ;
#11628 = VERTEX_POINT ( 'NONE', #15518 ) ;
#11629 = CARTESIAN_POINT ( 'NONE',  ( 5.568489401881125289, 48.03437091500646261, 90.41433880123798872 ) ) ;
#11630 = ADVANCED_FACE ( 'NONE', ( #20505 ), #14280, .F. ) ;
#11631 = CARTESIAN_POINT ( 'NONE',  ( -7.870013012521086537, 41.50220630618382245, 78.93669174070734584 ) ) ;
#11632 = CARTESIAN_POINT ( 'NONE',  ( -4.567115856812060670, 47.10047254335474065, 95.80496380123798872 ) ) ;
#11633 = VECTOR ( 'NONE', #14839, 1000.000000000000000 ) ;
#11634 = CARTESIAN_POINT ( 'NONE',  ( 8.598743959472566090, 42.74347214292002661, 79.23761354080345143 ) ) ;
#11635 = VERTEX_POINT ( 'NONE', #12532 ) ;
#11636 = CARTESIAN_POINT ( 'NONE',  ( -4.211488180634966660, 48.16625856408043660, 82.45433879953087342 ) ) ;
#11637 = ORIENTED_EDGE ( 'NONE', *, *, #19759, .T. ) ;
#11638 = DIRECTION ( 'NONE',  ( 0.007885122365275663500, 0.9999689119394085113, 1.805443505845543142E-16 ) ) ;
#11639 = CARTESIAN_POINT ( 'NONE',  ( 31.22215374030650281, 42.96218137147968008, 77.80433879953099563 ) ) ;
#11640 = DIRECTION ( 'NONE',  ( 1.540237394707284220E-16, 1.793354297423764243E-16, -1.000000000000000000 ) ) ;
#11641 = ORIENTED_EDGE ( 'NONE', *, *, #1633, .F. ) ;
#11642 = FACE_OUTER_BOUND ( 'NONE', #20083, .T. ) ;
#11643 = CARTESIAN_POINT ( 'NONE',  ( -3.566438244846302119, 38.23101125920473464, 78.58080938776616620 ) ) ;
#11644 = CARTESIAN_POINT ( 'NONE',  ( 2.916646314870772194, 38.79555996194921619, 92.55433879953098142 ) ) ;
#11645 = CARTESIAN_POINT ( 'NONE',  ( -1.477846259693495590, 47.62628298661744708, 61.15433879953099705 ) ) ;
#11646 = CARTESIAN_POINT ( 'NONE',  ( 0.3552956088218497954, 52.96739482532228749, 78.76353264627590534 ) ) ;
#11647 = ORIENTED_EDGE ( 'NONE', *, *, #9548, .F. ) ;
#11648 = CARTESIAN_POINT ( 'NONE',  ( -4.412197277429617870, 51.45204700985827628, 76.06958028623719770 ) ) ;
#11649 = VECTOR ( 'NONE', #9989, 1000.000000000000000 ) ;
#11650 = ORIENTED_EDGE ( 'NONE', *, *, #9928, .T. ) ;
#11651 = CARTESIAN_POINT ( 'NONE',  ( 1.652727357819363974, 35.35299279957455099, 79.45433879953087342 ) ) ;
#11652 = CARTESIAN_POINT ( 'NONE',  ( -6.841199144977723634, 40.72807414154878103, 77.45762758118813451 ) ) ;
#11653 = AXIS2_PLACEMENT_3D ( 'NONE', #11079, #19147, #11390 ) ;
#11654 = CARTESIAN_POINT ( 'NONE',  ( -4.535389824330220421, 37.70745443760639404, 77.32412050424863992 ) ) ;
#11655 = CARTESIAN_POINT ( 'NONE',  ( -3.226449543290803135, 47.76606447477306716, 95.05433879953076826 ) ) ;
#11656 = CARTESIAN_POINT ( 'NONE',  ( 2.463659247115867590, 38.82793883177424732, 91.62621379782397923 ) ) ;
#11657 = CARTESIAN_POINT ( 'NONE',  ( 5.454420194094963037, 37.61774161224509072, 76.04105433551922033 ) ) ;
#11658 = CARTESIAN_POINT ( 'NONE',  ( 4.199109002476567376, 47.83913663364971569, 95.05036078555451695 ) ) ;
#11659 = ORIENTED_EDGE ( 'NONE', *, *, #17628, .F. ) ;
#11660 = DIRECTION ( 'NONE',  ( 0.3165065846431827645, 0.9485903129789529098, 0.000000000000000000 ) ) ;
#11661 = CARTESIAN_POINT ( 'NONE',  ( 0.5221537403065045213, 39.16218137147969003, 94.60386871425484401 ) ) ;
#11662 = EDGE_CURVE ( 'NONE', #15850, #6157, #17889, .T. ) ;
#11663 = ORIENTED_EDGE ( 'NONE', *, *, #20256, .T. ) ;
#11664 = VECTOR ( 'NONE', #14637, 1000.000000000000000 ) ;
#11665 = DIRECTION ( 'NONE',  ( 0.000000000000000000, -1.000000000000000000, -2.168404344970984413E-15 ) ) ;
#11666 = LINE ( 'NONE', #258, #3114 ) ;
#11667 = CARTESIAN_POINT ( 'NONE',  ( -3.981178359372548492, 46.76218137147973408, 96.35183879953099506 ) ) ;
#11668 = ORIENTED_EDGE ( 'NONE', *, *, #7930, .F. ) ;
#11669 =( NAMED_UNIT ( * ) SI_UNIT ( $, .STERADIAN. ) SOLID_ANGLE_UNIT ( ) );
#11670 = CARTESIAN_POINT ( 'NONE',  ( -5.231921090767167826, 38.40807655202139870, 75.65168154244369703 ) ) ;
#11671 = MANIFOLD_SOLID_BREP ( 'Stock-MAS-160-1', #10208 ) ;
#11672 = EDGE_LOOP ( 'NONE', ( #4594, #686, #19755, #6388 ) ) ;
#11673 = CARTESIAN_POINT ( 'NONE',  ( 5.649834628789608182, 51.31498465973561451, 78.90029747732744170 ) ) ;
#11674 = CARTESIAN_POINT ( 'NONE',  ( 11.22215374030649926, 45.56218137147968861, 80.55433879953099563 ) ) ;
#11675 = CARTESIAN_POINT ( 'NONE',  ( 6.102441102155617969, 43.42752260303680600, 93.30496379953098085 ) ) ;
#11676 = ORIENTED_EDGE ( 'NONE', *, *, #8058, .F. ) ;
#11677 = CARTESIAN_POINT ( 'NONE',  ( -4.717426356068906479, 37.09203352051870439, 77.92182307551118470 ) ) ;
#11678 = EDGE_LOOP ( 'NONE', ( #8738, #4420, #9546, #5373 ) ) ;
#11679 = CARTESIAN_POINT ( 'NONE',  ( 1.514255888186008203, 51.36218137147968577, 48.36106904222365444 ) ) ;
#11680 = CARTESIAN_POINT ( 'NONE',  ( 4.199109002476567376, 47.83913663364971569, 93.80036078555450274 ) ) ;
#11681 = CARTESIAN_POINT ( 'NONE',  ( -3.350035803220276609, 49.20851703305431357, 94.47683880123798872 ) ) ;
#11682 = VECTOR ( 'NONE', #5078, 1000.000000000000000 ) ;
#11683 = LINE ( 'NONE', #5371, #18694 ) ;
#11684 = CARTESIAN_POINT ( 'NONE',  ( -7.202537930885374529, 41.41097462079392955, 78.61536821129558916 ) ) ;
#11685 = EDGE_LOOP ( 'NONE', ( #19826, #16149, #17855, #5043 ) ) ;
#11686 = CARTESIAN_POINT ( 'NONE',  ( 4.556677822976353376, 36.22933235006951946, 75.83703142516586126 ) ) ;
#11687 = DIRECTION ( 'NONE',  ( 1.000000000000000000, 0.000000000000000000, 0.000000000000000000 ) ) ;
#11688 = EDGE_CURVE ( 'NONE', #11453, #11104, #7743, .T. ) ;
#11689 = ORIENTED_EDGE ( 'NONE', *, *, #18796, .T. ) ;
#11690 = FACE_OUTER_BOUND ( 'NONE', #19675, .T. ) ;
#11691 = FACE_OUTER_BOUND ( 'NONE', #5910, .T. ) ;
#11692 = B_SPLINE_CURVE_WITH_KNOTS ( 'NONE', 3,
 ( #1830, #15225, #5208, #6810, #14894, #16504, #13316, #20097, #8417, #19788, #18099, #3520 ),
 .UNSPECIFIED., .F., .F.,
 ( 4, 2, 2, 2, 2, 4 ),
 ( 0.000000000000000000, 0.0001692975960979477246, 0.0003385951921958954493, 0.0004232439902448494572, 0.0005078927882938035192, 0.0006771903843916710942 ),
 .UNSPECIFIED. ) ;
#11693 = LINE ( 'NONE', #16575, #8202 ) ;
#11694 = CARTESIAN_POINT ( 'NONE',  ( -0.3080929418689875576, 37.85583172076933778, 93.85183880123797451 ) ) ;
#11695 = VERTEX_POINT ( 'NONE', #6339 ) ;
#11696 = ORIENTED_EDGE ( 'NONE', *, *, #16117, .F. ) ;
#11697 = VECTOR ( 'NONE', #5510, 1000.000000000000227 ) ;
#11698 = DIRECTION ( 'NONE',  ( 5.626130192357176673E-16, 1.831515347669941892E-30, -1.000000000000000000 ) ) ;
#11699 = ORIENTED_EDGE ( 'NONE', *, *, #2758, .F. ) ;
#11700 = CARTESIAN_POINT ( 'NONE',  ( -3.673304938980978651, 36.32078308949211731, 77.52205638859560111 ) ) ;
#11701 = EDGE_CURVE ( 'NONE', #12731, #15579, #9672, .T. ) ;
#11702 = FACE_OUTER_BOUND ( 'NONE', #8309, .T. ) ;
#11703 = LINE ( 'NONE', #17966, #15044 ) ;
#11704 = DIRECTION ( 'NONE',  ( 1.000000000000000000, 1.402518428993831676E-16, 0.000000000000000000 ) ) ;
#11705 = CARTESIAN_POINT ( 'NONE',  ( 0.6810009142495576651, 52.96482701376152136, 77.39848739855237625 ) ) ;
#11706 = EDGE_CURVE ( 'NONE', #15567, #16100, #1470, .T. ) ;
#11707 = DIRECTION ( 'NONE',  ( 1.000000000000000000, 1.402518428993842277E-16, 3.154042683594179442E-15 ) ) ;
#11708 = CARTESIAN_POINT ( 'NONE',  ( 0.5221537403065000804, 39.96218137147968719, 92.45433879953097289 ) ) ;
#11709 = CARTESIAN_POINT ( 'NONE',  ( -0.3080929418689875576, 37.85583172076933778, 93.69558880123800293 ) ) ;
#11710 = CARTESIAN_POINT ( 'NONE',  ( 5.568489401881125289, 48.03437091500646261, 94.16433880123797451 ) ) ;
#11711 = VERTEX_POINT ( 'NONE', #6761 ) ;
#11712 = ADVANCED_FACE ( 'NONE', ( #4952 ), #6554, .F. ) ;
#11713 = CARTESIAN_POINT ( 'NONE',  ( 5.316416202095706645, 37.50973464508803801, 75.36022115247205022 ) ) ;
#11714 = EDGE_CURVE ( 'NONE', #10035, #9413, #5159, .T. ) ;
#11715 = ADVANCED_FACE ( 'NONE', ( #3168 ), #3267, .F. ) ;
#11716 = ORIENTED_EDGE ( 'NONE', *, *, #12241, .T. ) ;
#11717 = CARTESIAN_POINT ( 'NONE',  ( 8.934486310075088866, 41.57094676672487310, 78.86350455626283917 ) ) ;
#11718 = CARTESIAN_POINT ( 'NONE',  ( 8.579938887586086693, 42.63956115774173838, 75.59610358210291281 ) ) ;
#11719 = FACE_OUTER_BOUND ( 'NONE', #17177, .T. ) ;
#11720 = CARTESIAN_POINT ( 'NONE',  ( 0.5221537403065097394, 44.16218137147969003, 92.55433879953098142 ) ) ;
#11721 = ADVANCED_FACE ( 'NONE', ( #19739 ), #11371, .F. ) ;
#11722 = CARTESIAN_POINT ( 'NONE',  ( 5.785641543149844246, 51.21466956273390991, 77.95070864408322109 ) ) ;
#11723 = ORIENTED_EDGE ( 'NONE', *, *, #7433, .F. ) ;
#11724 = CARTESIAN_POINT ( 'NONE',  ( 6.388813065772197319, 37.53850911581889704, 78.31663032931759005 ) ) ;
#11725 = CARTESIAN_POINT ( 'NONE',  ( 4.199109002476567376, 47.83913663364971569, 92.55433879953098142 ) ) ;
#11726 = CARTESIAN_POINT ( 'NONE',  ( 2.527576913102089762, 36.82540565608437078, 72.45433879953085921 ) ) ;
#11727 = ORIENTED_EDGE ( 'NONE', *, *, #15969, .F. ) ;
#11728 = APPLICATION_CONTEXT ( 'automotive_design' ) ;
#11729 = CARTESIAN_POINT ( 'NONE',  ( 8.373523562223194716, 41.80976150358770838, 76.25788209700408515 ) ) ;
#11730 = CARTESIAN_POINT ( 'NONE',  ( -4.559776018715441026, 36.97558356685869541, 78.86760481232144571 ) ) ;
#11731 = ORIENTED_EDGE ( 'NONE', *, *, #11244, .T. ) ;
#11732 = CARTESIAN_POINT ( 'NONE',  ( 3.460444912181559474, 49.25145096859824889, 92.99246380123798872 ) ) ;
#11733 = CARTESIAN_POINT ( 'NONE',  ( -7.247910519723778755, 41.56650193107834923, 78.91953837536544825 ) ) ;
#11734 = CARTESIAN_POINT ( 'NONE',  ( 3.460444912181559474, 49.25145096859824889, 95.49246380123798872 ) ) ;
#11735 = CARTESIAN_POINT ( 'NONE',  ( 8.951667845840693971, 41.62244091939069790, 77.14698585835439815 ) ) ;
#11736 = ORIENTED_EDGE ( 'NONE', *, *, #17243, .F. ) ;
#11737 = EDGE_CURVE ( 'NONE', #19622, #12696, #584, .T. ) ;
#11738 = CARTESIAN_POINT ( 'NONE',  ( 10.77494014480653917, 42.76218137147968434, 57.80715055817105252 ) ) ;
#11739 = ORIENTED_EDGE ( 'NONE', *, *, #7879, .T. ) ;
#11740 = DIRECTION ( 'NONE',  ( 1.540237394707284467E-16, 1.793354297423764243E-16, -1.000000000000000000 ) ) ;
#11741 = EDGE_CURVE ( 'NONE', #5518, #20901, #9983, .T. ) ;
#11742 = CARTESIAN_POINT ( 'NONE',  ( 6.828503391016846891, 43.33193468930419101, 95.25808880123800293 ) ) ;
#11743 = ORIENTED_EDGE ( 'NONE', *, *, #6245, .T. ) ;
#11744 = LINE ( 'NONE', #18952, #3838 ) ;
#11745 = DIRECTION ( 'NONE',  ( -0.5941461771851691553, -0.8043570849667760481, -2.357623395011396791E-16 ) ) ;
#11746 = CARTESIAN_POINT ( 'NONE',  ( 0.5221537403064985261, 44.16218137147969003, 96.05433879953096721 ) ) ;
#11747 = LINE ( 'NONE', #16633, #12542 ) ;
#11748 = CARTESIAN_POINT ( 'NONE',  ( 0.3721289191693305520, 52.35590880031470817, 78.82913797267801215 ) ) ;
#11749 = ORIENTED_EDGE ( 'NONE', *, *, #9410, .T. ) ;
#11750 = CARTESIAN_POINT ( 'NONE',  ( -4.044210365576157429, 50.96808155198777968, 76.14127734336351239 ) ) ;
#11751 = ORIENTED_EDGE ( 'NONE', *, *, #15451, .F. ) ;
#11752 = CARTESIAN_POINT ( 'NONE',  ( -3.154068805640487749, 36.83224912750022639, 78.04613744265782316 ) ) ;
#11753 = CARTESIAN_POINT ( 'NONE',  ( 25.85428507725097802, 26.43317006180084761, 75.00433879953101268 ) ) ;
#11754 = EDGE_CURVE ( 'NONE', #13741, #15505, #13077, .T. ) ;
#11755 = CARTESIAN_POINT ( 'NONE',  ( -4.160049236649933313, 37.43039271674265933, 76.90921114709620099 ) ) ;
#11756 = CARTESIAN_POINT ( 'NONE',  ( 4.512269934384614878, 47.81844922806527620, 92.56371379611699979 ) ) ;
#11757 = CARTESIAN_POINT ( 'NONE',  ( -4.812088799398940075, 42.22067586467031930, 95.06371379782397923 ) ) ;
#11758 = CARTESIAN_POINT ( 'NONE',  ( 5.847829093480187979, 37.15194177590640834, 76.49330797698027595 ) ) ;
#11759 = CARTESIAN_POINT ( 'NONE',  ( -4.621776214648809500, 51.30228957449607208, 75.36056307228784590 ) ) ;
#11760 = ORIENTED_EDGE ( 'NONE', *, *, #17036, .F. ) ;
#11761 = CARTESIAN_POINT ( 'NONE',  ( 1.205864535894263900, 52.96136243468175309, 79.49721971971477785 ) ) ;
#11762 = CARTESIAN_POINT ( 'NONE',  ( 5.450944860649778789, 36.86834283398499679, 78.16244716952144245 ) ) ;
#11763 = ORIENTED_EDGE ( 'NONE', *, *, #10136, .F. ) ;
#11764 = DIRECTION ( 'NONE',  ( 0.5941461771841298756, 0.8043570849675437673, -3.462188797834771445E-14 ) ) ;
#11765 = DIRECTION ( 'NONE',  ( -0.02533578529877045238, -0.9996789974703352843, -1.831801750099146688E-16 ) ) ;
#11766 = CARTESIAN_POINT ( 'NONE',  ( -5.058133621542618030, 44.89684013992257405, 95.17996379953099506 ) ) ;
#11767 = B_SPLINE_SURFACE_WITH_KNOTS ( 'NONE', 3, 1, ( 
 ( #15804, #12402 ),
 ( #18779, #14184 ),
 ( #12494, #4194 ),
 ( #18881, #4289 ),
 ( #20664, #13773 ),
 ( #10815, #20246 ),
 ( #17281, #2706 ),
 ( #9213, #14089 ),
 ( #6098, #18980 ),
 ( #2814, #4392 ),
 ( #12603, #10917 ),
 ( #17387, #11020 ),
 ( #17490, #15902 ),
 ( #18010, #9414 ),
 ( #13119, #12704 ),
 ( #6513, #12910 ),
 ( #6300, #12800 ),
 ( #3015, #1322 ),
 ( #3124, #7807 ),
 ( #9728, #9521 ),
 ( #19182, #17587 ),
 ( #6613, #4595 ),
 ( #20768, #14608 ),
 ( #16209, #6202 ),
 ( #4908, #9626 ),
 ( #6403, #13019 ),
 ( #11119, #9830 ) ),
 .UNSPECIFIED., .F., .F., .F.,
 ( 4, 1, 1, 1, 1, 1, 1, 1, 1, 1, 1, 1, 1, 1, 1, 1, 1, 1, 1, 1, 1, 1, 1, 1, 4 ),
 ( 2, 2 ),
 ( 0.000000000000000000, 0.08415130211954198469, 0.1639620550106605512, 0.2403084560778752377, 0.3136616503690570767, 0.3487238096526073527, 0.3821668720153286181, 0.4136737894986983743, 0.4437099131648768457, 0.4722505124987256275, 0.4989577201472497614, 0.5245780966751731889, 0.5489676856186370690, 0.5954867311152326481, 0.6405007172309487018, 0.6844907576478919120, 0.7283883565803446203, 0.7516682776372889396, 0.7779555554382332483, 0.8073737814008299374, 0.8396655338036946858, 0.8751296329422569853, 0.9135058715745314473, 0.9551265033309996877, 1.000000000000000000 ),
 ( 0.000000000000000000, 1.000000000000000000 ),
 .UNSPECIFIED. ) ;
#11768 = VERTEX_POINT ( 'NONE', #9875 ) ;
#11769 = CARTESIAN_POINT ( 'NONE',  ( -4.608840676074902554, 37.94783214889832124, 75.38158877174898009 ) ) ;
#11770 = EDGE_LOOP ( 'NONE', ( #15624, #15018, #19276, #5269 ) ) ;
#11771 = CARTESIAN_POINT ( 'NONE',  ( 6.012275498921958672, 37.26944915646792822, 78.37198585835440667 ) ) ;
#11772 = LINE ( 'NONE', #6650, #1003 ) ;
#11773 = EDGE_LOOP ( 'NONE', ( #20539, #19319, #574, #18170 ) ) ;
#11774 = CARTESIAN_POINT ( 'NONE',  ( -4.155425753337090633, 37.45166743282118915, 78.17872471894986575 ) ) ;
#11775 = CARTESIAN_POINT ( 'NONE',  ( 3.460444912181559474, 49.25145096859824889, 94.39871380123798872 ) ) ;
#11776 = EDGE_LOOP ( 'NONE', ( #9286, #3147, #3362, #16905 ) ) ;
#11777 = FACE_OUTER_BOUND ( 'NONE', #9397, .T. ) ;
#11778 = CARTESIAN_POINT ( 'NONE',  ( 0.6888015158513324243, 52.96107022024632727, 75.36125108926063376 ) ) ;
#11779 = VECTOR ( 'NONE', #14480, 1000.000000000000000 ) ;
#11780 = DIRECTION ( 'NONE',  ( 0.000000000000000000, 0.000000000000000000, 1.000000000000000000 ) ) ;
#11781 = CARTESIAN_POINT ( 'NONE',  ( 5.553908412425695218, 50.63686217341278706, 77.18328619514350919 ) ) ;
#11782 = CARTESIAN_POINT ( 'NONE',  ( -7.880212061628153464, 41.54679441531448703, 76.16022115247204738 ) ) ;
#11783 = ORIENTED_EDGE ( 'NONE', *, *, #11282, .F. ) ;
#11784 = ORIENTED_EDGE ( 'NONE', *, *, #5425, .T. ) ;
#11785 = CARTESIAN_POINT ( 'NONE',  ( 4.449581223279069242, 37.07258062326099690, 75.53067132529541539 ) ) ;
#11786 = CARTESIAN_POINT ( 'NONE',  ( 7.690906676071723069, 40.20827776290879285, 78.77723610448765612 ) ) ;
#11787 = ORIENTED_EDGE ( 'NONE', *, *, #2977, .T. ) ;
#11788 = DIRECTION ( 'NONE',  ( 1.000000000000000000, -1.110223024625156540E-16, 1.779391786395883043E-16 ) ) ;
#11789 = LINE ( 'NONE', #8491, #1074 ) ;
#11790 = CARTESIAN_POINT ( 'NONE',  ( -5.154188915835984375, 42.64120994080404614, 93.61746380123797451 ) ) ;
#11791 = ORIENTED_EDGE ( 'NONE', *, *, #1603, .F. ) ;
#11792 = ORIENTED_EDGE ( 'NONE', *, *, #16808, .T. ) ;
#11793 = AXIS2_PLACEMENT_3D ( 'NONE', #19680, #1614, #8416 ) ;
#11794 = CARTESIAN_POINT ( 'NONE',  ( 6.416710426036811299, 49.83450939472239583, 78.95155228521747404 ) ) ;
#11795 = ORIENTED_EDGE ( 'NONE', *, *, #13883, .F. ) ;
#11796 = CARTESIAN_POINT ( 'NONE',  ( 5.552491339591165698, 50.63796333333529986, 76.08571115608103241 ) ) ;
#11797 = CARTESIAN_POINT ( 'NONE',  ( 7.962360810970000813, 41.03860973493735997, 75.42295143068700725 ) ) ;
#11798 = CARTESIAN_POINT ( 'NONE',  ( -4.032264951078913029, 50.98107207184723677, 78.45066232894264147 ) ) ;
#11799 = DIRECTION ( 'NONE',  ( 0.3165065846431827645, 0.9485903129789529098, 0.000000000000000000 ) ) ;
#11800 = EDGE_CURVE ( 'NONE', #14895, #15118, #5058, .T. ) ;
#11801 = CARTESIAN_POINT ( 'NONE',  ( 0.5221537403065010796, 44.16218137147969003, 77.84651775085080772 ) ) ;
#11802 = CARTESIAN_POINT ( 'NONE',  ( 8.801580714196775901, 41.17262026450377022, 76.07953452682116335 ) ) ;
#11803 = FACE_OUTER_BOUND ( 'NONE', #12661, .T. ) ;
#11804 = DIRECTION ( 'NONE',  ( -1.084202172485505420E-16, -1.000000000000000000, 0.000000000000000000 ) ) ;
#11805 = CARTESIAN_POINT ( 'NONE',  ( 3.460444912181559474, 49.25145096859824889, 90.49246380123798872 ) ) ;
#11806 = VECTOR ( 'NONE', #4867, 1000.000000000000114 ) ;
#11807 = CARTESIAN_POINT ( 'NONE',  ( -7.370301013496298737, 41.95215886586026954, 78.67381781145438424 ) ) ;
#11808 = LINE ( 'NONE', #305, #1057 ) ;
#11809 = ORIENTED_EDGE ( 'NONE', *, *, #5232, .T. ) ;
#11810 = DIRECTION ( 'NONE',  ( 0.3165065846431827645, 0.9485903129789529098, 0.000000000000000000 ) ) ;
#11811 = EDGE_CURVE ( 'NONE', #18002, #4756, #8371, .T. ) ;
#11812 = PLANE ( 'NONE',  #16719 ) ;
#11813 = LINE ( 'NONE', #13609, #9238 ) ;
#11814 = CARTESIAN_POINT ( 'NONE',  ( 4.987494971863720927, 47.58855820898865829, 90.96121379953099506 ) ) ;
#11815 = AXIS2_PLACEMENT_3D ( 'NONE', #9641, #12922, #1159 ) ;
#11816 = CARTESIAN_POINT ( 'NONE',  ( 29.03948732994507864, 45.16218137147969003, 74.70433879953100131 ) ) ;
#11817 = LINE ( 'NONE', #13722, #8596 ) ;
#11818 = EDGE_CURVE ( 'NONE', #13327, #3871, #15203, .T. ) ;
#11819 = ORIENTED_EDGE ( 'NONE', *, *, #6591, .F. ) ;
#11820 = VERTEX_POINT ( 'NONE', #1843 ) ;
#11821 = VECTOR ( 'NONE', #18703, 1000.000000000000114 ) ;
#11822 = CARTESIAN_POINT ( 'NONE',  ( 8.265572330772934961, 41.46143766428760813, 79.54654421141340492 ) ) ;
#11823 = CARTESIAN_POINT ( 'NONE',  ( -4.716387082485073989, 37.09126585098686490, 75.36022115247205022 ) ) ;
#11824 = LINE ( 'NONE', #18299, #1796 ) ;
#11825 = VERTEX_POINT ( 'NONE', #2044 ) ;
#11826 = EDGE_CURVE ( 'NONE', #10614, #11899, #7025, .T. ) ;
#11827 = CARTESIAN_POINT ( 'NONE',  ( 5.755371611800503828, 51.23702874167446453, 77.28963291717792572 ) ) ;
#11828 = CARTESIAN_POINT ( 'NONE',  ( -4.689916854477826469, 37.07171335984372718, 78.93589701864812014 ) ) ;
#11829 = CARTESIAN_POINT ( 'NONE',  ( -3.981178359372548492, 46.76218137147973408, 92.91433880294496817 ) ) ;
#11830 = AXIS2_PLACEMENT_3D ( 'NONE', #12172, #17063, #17164 ) ;
#11831 = CARTESIAN_POINT ( 'NONE',  ( 1.994229309409025097, 52.20255399867006929, 77.17808573571203112 ) ) ;
#11832 = EDGE_CURVE ( 'NONE', #4650, #19160, #16421, .T. ) ;
#11833 = CARTESIAN_POINT ( 'NONE',  ( -3.350035803220276609, 49.20851703305431357, 94.47683880123798872 ) ) ;
#11834 = CARTESIAN_POINT ( 'NONE',  ( -3.716800330428160049, 36.35291138305289849, 77.85659439586764563 ) ) ;
#11835 = B_SPLINE_CURVE_WITH_KNOTS ( 'NONE', 3,
 ( #19815, #10158, #16640, #5237, #10269, #11752, #19915, #11852, #2377, #3548 ),
 .UNSPECIFIED., .F., .F.,
 ( 4, 2, 2, 2, 4 ),
 ( 0.000000000000000000, 0.0002565823024332847865, 0.0005131646048665695729, 0.0007697469072998543594, 0.001026329209733139146 ),
 .UNSPECIFIED. ) ;
#11836 = CARTESIAN_POINT ( 'NONE',  ( -8.189734885440142165, 42.91998662985088941, 78.64696458830286474 ) ) ;
#11837 = ORIENTED_EDGE ( 'NONE', *, *, #3859, .T. ) ;
#11838 = DIRECTION ( 'NONE',  ( -1.540237394707284220E-16, -1.793354297423764243E-16, 1.000000000000000000 ) ) ;
#11839 = VERTEX_POINT ( 'NONE', #6822 ) ;
#11840 = CARTESIAN_POINT ( 'NONE',  ( -7.720485820677993161, 47.24421020474736110, 77.98042076123601873 ) ) ;
#11841 = CARTESIAN_POINT ( 'NONE',  ( -0.9988176903691428077, 49.83852402762217082, 91.89871380123798872 ) ) ;
#11842 = ORIENTED_EDGE ( 'NONE', *, *, #12121, .F. ) ;
#11843 = CARTESIAN_POINT ( 'NONE',  ( 1.630627053521184200, 49.16218137147969003, 92.68365272277780775 ) ) ;
#11844 = VECTOR ( 'NONE', #15273, 1000.000000000000000 ) ;
#11845 = DIRECTION ( 'NONE',  ( -1.334402673828313832E-16, 2.891205793294680792E-16, 1.000000000000000000 ) ) ;
#11846 = CARTESIAN_POINT ( 'NONE',  ( -4.092737432821778931, 51.68032131864361389, 79.48422614141084352 ) ) ;
#11847 = CARTESIAN_POINT ( 'NONE',  ( -4.884656273474450749, 44.39824779480852612, 93.34496379953098710 ) ) ;
#11848 = ORIENTED_EDGE ( 'NONE', *, *, #5834, .T. ) ;
#11849 = EDGE_CURVE ( 'NONE', #14474, #880, #1935, .T. ) ;
#11850 = CARTESIAN_POINT ( 'NONE',  ( 5.241460166982748525, 50.86801069014953924, 78.30875056423674607 ) ) ;
#11851 = ORIENTED_EDGE ( 'NONE', *, *, #20141, .T. ) ;
#11852 = CARTESIAN_POINT ( 'NONE',  ( -3.103229033235510581, 36.80712667557776285, 78.29630717499995285 ) ) ;
#11853 = EDGE_CURVE ( 'NONE', #14499, #347, #13329, .T. ) ;
#11854 = CARTESIAN_POINT ( 'NONE',  ( -6.756808310619874192, 40.46120382059411469, 77.87635769503857830 ) ) ;
#11855 = CARTESIAN_POINT ( 'NONE',  ( -7.294472080575377326, 41.68420623513899415, 78.93669174070734584 ) ) ;
#11856 = CARTESIAN_POINT ( 'NONE',  ( -7.674265136008432187, 40.95548271059750078, 76.88066623382401588 ) ) ;
#11857 = CARTESIAN_POINT ( 'NONE',  ( 5.856396280011940902, 46.10368687828906076, 92.09496379782399345 ) ) ;
#11858 = CARTESIAN_POINT ( 'NONE',  ( 5.843112203128086435, 37.14857125875717969, 76.21413800766271152 ) ) ;
#11859 = EDGE_CURVE ( 'NONE', #7741, #14613, #5431, .T. ) ;
#11860 = CIRCLE ( 'NONE', #5381, 3.999999999999996447 ) ;
#11861 = EDGE_CURVE ( 'NONE', #1174, #19686, #19131, .T. ) ;
#11862 = ORIENTED_EDGE ( 'NONE', *, *, #14396, .T. ) ;
#11863 = LINE ( 'NONE', #5349, #18677 ) ;
#11864 = CARTESIAN_POINT ( 'NONE',  ( 5.518796429342951448, 36.91682708076865538, 78.21801395346943764 ) ) ;
#11865 = VERTEX_POINT ( 'NONE', #11947 ) ;
#11866 = CARTESIAN_POINT ( 'NONE',  ( -3.154801521863568325, 47.83913663364971569, 93.80036078214054385 ) ) ;
#11867 = CARTESIAN_POINT ( 'NONE',  ( 1.256812508749381774, 49.74246873332880625, 93.61746379953098085 ) ) ;
#11868 = CARTESIAN_POINT ( 'NONE',  ( 1.256812508749381774, 49.74246873332880625, 92.36746379953098085 ) ) ;
#11869 = ORIENTED_EDGE ( 'NONE', *, *, #5062, .F. ) ;
#11870 = CARTESIAN_POINT ( 'NONE',  ( 8.793292705229012185, 41.14778057584590698, 77.83369646723784285 ) ) ;
#11871 = DIRECTION ( 'NONE',  ( -1.000000000000000000, 0.000000000000000000, 0.000000000000000000 ) ) ;
#11872 = VERTEX_POINT ( 'NONE', #16730 ) ;
#11873 = CARTESIAN_POINT ( 'NONE',  ( 23.63948732994508717, 45.16218137147969003, 74.70433879953098710 ) ) ;
#11874 = CARTESIAN_POINT ( 'NONE',  ( 1.087740465381641375, 52.94398708878058102, 76.77198585835439815 ) ) ;
#11875 = ORIENTED_EDGE ( 'NONE', *, *, #1581, .T. ) ;
#11876 = CARTESIAN_POINT ( 'NONE',  ( -4.681776609547218193, 37.06570048882251456, 77.92992558049613194 ) ) ;
#11877 = VECTOR ( 'NONE', #6617, 1000.000000000000000 ) ;
#11878 = CARTESIAN_POINT ( 'NONE',  ( 5.568489401881125289, 48.03437091500646261, 94.32058880123798872 ) ) ;
#11879 = VERTEX_POINT ( 'NONE', #5222 ) ;
#11880 = CARTESIAN_POINT ( 'NONE',  ( 0.7328066911292444585, 52.35949871758720775, 77.42541623458531319 ) ) ;
#11881 = CARTESIAN_POINT ( 'NONE',  ( 2.112743662072855688, 52.81725452181535019, 76.30775568555031896 ) ) ;
#11882 = CARTESIAN_POINT ( 'NONE',  ( 10.77494014480653917, 42.96218137147968008, 57.80715055817105252 ) ) ;
#11883 = AXIS2_PLACEMENT_3D ( 'NONE', #19922, #6742, #13247 ) ;
#11884 = SHAPE_REPRESENTATION_RELATIONSHIP ( 'NONE' , 'NONE' ,  #14198, #10379 ) ;
#11885 = EDGE_CURVE ( 'NONE', #8267, #13025, #16518, .T. ) ;
#11886 = CARTESIAN_POINT ( 'NONE',  ( 6.645808250425207397, 50.57929906569810896, 75.61685692759286326 ) ) ;
#11887 = CARTESIAN_POINT ( 'NONE',  ( 5.928963754087450688, 43.92611494815086814, 93.96996379953098710 ) ) ;
#11888 = VECTOR ( 'NONE', #8150, 1000.000000000000000 ) ;
#11889 = B_SPLINE_CURVE_WITH_KNOTS ( 'NONE', 3,
 ( #3275, #6351, #9888, #11066, #12655, #17536, #6457, #11482, #9466, #1373, #7861, #16369 ),
 .UNSPECIFIED., .F., .F.,
 ( 4, 2, 2, 2, 2, 4 ),
 ( 0.000000000000000000, 0.0003548653088398171624, 0.0004435816360497409462, 0.0005322979632596647843, 0.0006210142904695885140, 0.0007097306176795123520 ),
 .UNSPECIFIED. ) ;
#11890 = CARTESIAN_POINT ( 'NONE',  ( 2.350558581813038117, 49.87752504164859602, 69.32593395802446423 ) ) ;
#11891 = VERTEX_POINT ( 'NONE', #18425 ) ;
#11892 = ORIENTED_EDGE ( 'NONE', *, *, #14549, .F. ) ;
#11893 = CARTESIAN_POINT ( 'NONE',  ( 0.5221537403065005245, 44.16218137147968292, 82.45433879953087342 ) ) ;
#11894 = VECTOR ( 'NONE', #3683, 1000.000000000000000 ) ;
#11895 = ORIENTED_EDGE ( 'NONE', *, *, #16156, .T. ) ;
#11896 = CARTESIAN_POINT ( 'NONE',  ( 11.22215374030649926, 51.36218137147968577, 80.55433879953099563 ) ) ;
#11897 = CARTESIAN_POINT ( 'NONE',  ( 0.3403435922581479200, 52.35615943634957858, 77.57937361552639288 ) ) ;
#11898 = CARTESIAN_POINT ( 'NONE',  ( -6.709328582052544121, 40.29621921162755172, 72.45433879953085921 ) ) ;
#11899 = VERTEX_POINT ( 'NONE', #3842 ) ;
#11900 = EDGE_LOOP ( 'NONE', ( #17723, #3994, #3864, #10268, #7524, #3351 ) ) ;
#11901 = VECTOR ( 'NONE', #19189, 1000.000000000000227 ) ;
#11902 = VECTOR ( 'NONE', #7959, 1000.000000000000227 ) ;
#11903 = DIRECTION ( 'NONE',  ( -0.9534635866061451637, -0.3015081906286224411, -2.009271279954815058E-16 ) ) ;
#11904 = ORIENTED_EDGE ( 'NONE', *, *, #19154, .T. ) ;
#11905 = CARTESIAN_POINT ( 'NONE',  ( 5.459413332645724815, 50.70932733642038670, 75.97917348163453255 ) ) ;
#11906 = CARTESIAN_POINT ( 'NONE',  ( 0.3908531827224452360, 52.96817599631071261, 75.36353278631986541 ) ) ;
#11907 = PLANE ( 'NONE',  #3282 ) ;
#11908 = CARTESIAN_POINT ( 'NONE',  ( 5.076572431691917409, 37.34329067111212197, 76.70433879953087342 ) ) ;
#11909 = LINE ( 'NONE', #3694, #16068 ) ;
#11910 = CARTESIAN_POINT ( 'NONE',  ( 1.352400422481993658, 50.46853102219002096, 94.47683880123798872 ) ) ;
#11911 = VECTOR ( 'NONE', #20909, 1000.000000000000000 ) ;
#11912 = CARTESIAN_POINT ( 'NONE',  ( 0.8500593474157197571, 52.96349392588599869, 77.74134350746754762 ) ) ;
#11913 = VECTOR ( 'NONE', #9437, 1000.000000000000000 ) ;
#11914 = PLANE ( 'NONE',  #7802 ) ;
#11915 = PLANE ( 'NONE',  #19043 ) ;
#11916 = B_SPLINE_CURVE_WITH_KNOTS ( 'NONE', 3,
 ( #20368, #5804, #20157, #1017, #2613, #9113, #15600, #5587, #12092, #15814, #18891, #9640 ),
 .UNSPECIFIED., .F., .F.,
 ( 4, 2, 2, 2, 2, 4 ),
 ( 0.000000000000000000, 0.0004479885639438729037, 0.0005599857049298308026, 0.0006719828459157885930, 0.0007839799869017464919, 0.0008959771278877043908 ),
 .UNSPECIFIED. ) ;
#11917 = CARTESIAN_POINT ( 'NONE',  ( -5.154188915835984375, 42.64120994080404614, 92.21121380123797451 ) ) ;
#11918 = VECTOR ( 'NONE', #19930, 999.9999999999998863 ) ;
#11919 = DIRECTION ( 'NONE',  ( -1.779391786395883536E-16, -5.922860397471806844E-17, 1.000000000000000000 ) ) ;
#11920 = CARTESIAN_POINT ( 'NONE',  ( 0.4126924915616977940, 52.96692776651367751, 76.01942718764288998 ) ) ;
#11921 = ORIENTED_EDGE ( 'NONE', *, *, #17153, .T. ) ;
#11922 = CARTESIAN_POINT ( 'NONE',  ( 5.327820932109281316, 50.80650718277960465, 77.28232693284115840 ) ) ;
#11923 = DIRECTION ( 'NONE',  ( -0.5941461771851691553, -0.8043570849667760481, -2.357623395011396791E-16 ) ) ;
#11924 = CARTESIAN_POINT ( 'NONE',  ( -4.895465483855350186, 37.22354385236106822, 78.55727908454632313 ) ) ;
#11925 = CARTESIAN_POINT ( 'NONE',  ( -0.9988176903691428077, 49.83852402762217082, 92.05496380123798872 ) ) ;
#11926 = ADVANCED_FACE ( 'NONE', ( #16622 ), #8540, .T. ) ;
#11927 = CARTESIAN_POINT ( 'NONE',  ( -4.517625420443597939, 36.94444861784495515, 76.85096240152589075 ) ) ;
#11928 = FACE_OUTER_BOUND ( 'NONE', #5221, .T. ) ;
#11929 = CARTESIAN_POINT ( 'NONE',  ( 28.52215374030649642, 44.16218137147969003, 87.85433879953103542 ) ) ;
#11930 = ORIENTED_EDGE ( 'NONE', *, *, #16493, .T. ) ;
#11931 = EDGE_LOOP ( 'NONE', ( #21002, #7270, #7998, #7258 ) ) ;
#11932 = CARTESIAN_POINT ( 'NONE',  ( 6.403524027200472091, 49.87623753264638538, 77.45731366823912367 ) ) ;
#11933 = CARTESIAN_POINT ( 'NONE',  ( -7.949137504989498559, 41.77948864320536160, 78.13669174070733447 ) ) ;
#11934 = CARTESIAN_POINT ( 'NONE',  ( -4.166541536208259622, 37.43491202974078647, 78.74462879972740836 ) ) ;
#11935 = EDGE_LOOP ( 'NONE', ( #19461, #18154, #61, #4166, #17261, #13633, #1463, #14923, #20496, #4465, #15348, #9159 ) ) ;
#11936 = DIRECTION ( 'NONE',  ( 0.000000000000000000, -1.000000000000000000, 0.000000000000000000 ) ) ;
#11937 = CARTESIAN_POINT ( 'NONE',  ( -4.335999953777515792, 46.33399087051191145, 95.05433879953096721 ) ) ;
#11938 = ADVANCED_FACE ( 'NONE', ( #8327 ), #6714, .F. ) ;
#11939 = LINE ( 'NONE', #642, #10556 ) ;
#11940 = CARTESIAN_POINT ( 'NONE',  ( 6.102441102155617969, 43.42752260303680600, 92.36746380294498238 ) ) ;
#11941 = CARTESIAN_POINT ( 'NONE',  ( 3.460444912181559474, 49.25145096859824889, 94.24246380123798872 ) ) ;
#11942 = CARTESIAN_POINT ( 'NONE',  ( -7.816556923607321572, 41.33316136529717966, 78.89406302991613984 ) ) ;
#11943 = CARTESIAN_POINT ( 'NONE',  ( -4.524181921268124462, 40.28999182795290324, 93.53933880123797451 ) ) ;
#11944 = PRODUCT_DEFINITION_SHAPE ( 'NONE', 'NONE',  #21041 ) ;
#11945 = DIRECTION ( 'NONE',  ( 0.5813877811927012917, -0.8136266022444372803, -5.636455622144620416E-17 ) ) ;
#11946 = ORIENTED_EDGE ( 'NONE', *, *, #2246, .T. ) ;
#11947 = CARTESIAN_POINT ( 'NONE',  ( 2.122153740306508496, 47.82824192744436687, 77.55433879953099563 ) ) ;
#11948 = EDGE_LOOP ( 'NONE', ( #3686, #6885, #15707, #20093 ) ) ;
#11949 = AXIS2_PLACEMENT_3D ( 'NONE', #13634, #226, #19997 ) ;
#11950 = CARTESIAN_POINT ( 'NONE',  ( -4.804325902087982492, 51.17184625142267151, 78.52518475144754007 ) ) ;
#11951 = VECTOR ( 'NONE', #10467, 1000.000000000000227 ) ;
#11952 = CARTESIAN_POINT ( 'NONE',  ( 6.828503391016846891, 43.33193468930419101, 90.25808880123800293 ) ) ;
#11953 = VERTEX_POINT ( 'NONE', #5322 ) ;
#11954 = CARTESIAN_POINT ( 'NONE',  ( 6.705715917364262424, 48.58072850854415492, 75.45433879953087342 ) ) ;
#11955 = CARTESIAN_POINT ( 'NONE',  ( -2.055347584452832166, 51.31805217249780782, 72.45433879953087342 ) ) ;
#11956 = DIRECTION ( 'NONE',  ( -0.7071067811865435759, -0.7071067811865515695, -0.000000000000000000 ) ) ;
#11957 = CARTESIAN_POINT ( 'NONE',  ( 5.581406744796362673, 50.61539444998253856, 76.38301527011910252 ) ) ;
#11958 = CARTESIAN_POINT ( 'NONE',  ( 5.223270137239985011, 50.87543472457460325, 77.16202479023476712 ) ) ;
#11959 = CARTESIAN_POINT ( 'NONE',  ( -0.5863195729081815966, 39.16218137147969003, 93.62115272619176665 ) ) ;
#11960 = ORIENTED_EDGE ( 'NONE', *, *, #19710, .T. ) ;
#11961 = CARTESIAN_POINT ( 'NONE',  ( 8.221632462510044093, 41.34112525087960677, 77.36736982993747347 ) ) ;
#11962 = EDGE_CURVE ( 'NONE', #492, #3468, #8429, .T. ) ;
#11963 = ORIENTED_EDGE ( 'NONE', *, *, #11688, .F. ) ;
#11964 = CARTESIAN_POINT ( 'NONE',  ( -0.4699484075730043786, 51.36218137147968577, 52.53721119516358584 ) ) ;
#11965 = CARTESIAN_POINT ( 'NONE',  ( 6.569564547327074955, 50.63561721789299952, 77.67636243622263237 ) ) ;
#11966 = CARTESIAN_POINT ( 'NONE',  ( 4.394343283833276104, 39.11584570990505938, 92.75808880123797451 ) ) ;
#11967 = EDGE_CURVE ( 'NONE', #1387, #8963, #13637, .T. ) ;
#11968 = VECTOR ( 'NONE', #10385, 1000.000000000000114 ) ;
#11969 = CARTESIAN_POINT ( 'NONE',  ( -4.812088799398938299, 42.22067586467031930, 91.46996379782397923 ) ) ;
#11970 = FACE_OUTER_BOUND ( 'NONE', #767, .T. ) ;
#11971 = AXIS2_PLACEMENT_3D ( 'NONE', #7755, #1374, #1061 ) ;
#11972 = ORIENTED_EDGE ( 'NONE', *, *, #8470, .F. ) ;
#11973 = DIRECTION ( 'NONE',  ( -1.000000000000000000, -1.402518428993831183E-16, 7.152522014899634076E-33 ) ) ;
#11974 = EDGE_CURVE ( 'NONE', #16856, #6568, #14091, .T. ) ;
#11975 = ORIENTED_EDGE ( 'NONE', *, *, #4153, .T. ) ;
#11976 = LINE ( 'NONE', #18876, #11231 ) ;
#11977 = EDGE_CURVE ( 'NONE', #3866, #19468, #2153, .T. ) ;
#11978 = CARTESIAN_POINT ( 'NONE',  ( -2.904223097202481174, 48.62752260303690122, 96.27371379953099506 ) ) ;
#11979 = CARTESIAN_POINT ( 'NONE',  ( 5.025485839985549319, 41.56218137147963887, 95.72683879953099506 ) ) ;
#11980 = CARTESIAN_POINT ( 'NONE',  ( -7.332176014465951575, 42.24478606644824907, 77.21863129581211638 ) ) ;
#11981 = ORIENTED_EDGE ( 'NONE', *, *, #15762, .T. ) ;
#11982 = LINE ( 'NONE', #2182, #7842 ) ;
#11983 = FACE_BOUND ( 'NONE', #11369, .T. ) ;
#11984 = VERTEX_POINT ( 'NONE', #16834 ) ;
#11985 = VECTOR ( 'NONE', #14651, 1000.000000000000114 ) ;
#11986 = DIRECTION ( 'NONE',  ( -0.5941461771851693774, -0.8043570849667760481, -2.357623395011396791E-16 ) ) ;
#11987 = LINE ( 'NONE', #18783, #15631 ) ;
#11988 = EDGE_CURVE ( 'NONE', #16102, #4359, #2252, .T. ) ;
#11989 = CARTESIAN_POINT ( 'NONE',  ( -3.981178359372548492, 46.76218137147973408, 91.35183879953098085 ) ) ;
#11990 = CIRCLE ( 'NONE', #5155, 8.199999999999999289 ) ;
#11991 = EDGE_CURVE ( 'NONE', #7324, #20830, #8750, .T. ) ;
#11992 = ORIENTED_EDGE ( 'NONE', *, *, #19596, .F. ) ;
#11993 = DIRECTION ( 'NONE',  ( -0.9485903129789527988, 0.3165065846431829311, -8.934458285744989980E-17 ) ) ;
#11994 = ORIENTED_EDGE ( 'NONE', *, *, #18363, .F. ) ;
#11995 = CARTESIAN_POINT ( 'NONE',  ( -4.477846259693498254, 36.96218137147968008, 54.55433879953098852 ) ) ;
#11996 = DIRECTION ( 'NONE',  ( 0.9485903129789529098, -0.3165065846431826535, 8.934458285744997376E-17 ) ) ;
#11997 = EDGE_CURVE ( 'NONE', #8922, #20886, #3424, .T. ) ;
#11998 = CARTESIAN_POINT ( 'NONE',  ( -0.9988176903691428077, 49.83852402762217082, 90.64871380123798872 ) ) ;
#11999 = SHAPE_DEFINITION_REPRESENTATION ( #15161, #7678 ) ;
#12000 = CARTESIAN_POINT ( 'NONE',  ( -4.481786250374327985, 37.67261160860749669, 76.00936707281648808 ) ) ;
#12001 = CARTESIAN_POINT ( 'NONE',  ( -1.477846259693492481, 50.16218137147969713, 66.55433879953099563 ) ) ;
#12002 = VECTOR ( 'NONE', #15903, 1000.000000000000114 ) ;
#12003 = CARTESIAN_POINT ( 'NONE',  ( -3.853146778511270742, 37.22459720243209347, 79.49239465720451392 ) ) ;
#12004 = CIRCLE ( 'NONE', #2438, 17.99999999999999645 ) ;
#12005 = ORIENTED_EDGE ( 'NONE', *, *, #5435, .T. ) ;
#12006 = VERTEX_POINT ( 'NONE', #18634 ) ;
#12007 = CARTESIAN_POINT ( 'NONE',  ( -4.895593109503407980, 37.22363812428621088, 78.53742703482498655 ) ) ;
#12008 = ORIENTED_EDGE ( 'NONE', *, *, #1803, .F. ) ;
#12009 = DIRECTION ( 'NONE',  ( 6.308085367188358884E-15, 3.469446951953626515E-16, 1.000000000000000000 ) ) ;
#12010 = CARTESIAN_POINT ( 'NONE',  ( 0.4298316049500268132, 52.96680757607156664, 77.42486900944150818 ) ) ;
#12011 = DIRECTION ( 'NONE',  ( 1.540237394707284220E-16, 1.793354297423764243E-16, -1.000000000000000000 ) ) ;
#12012 = ORIENTED_EDGE ( 'NONE', *, *, #3960, .T. ) ;
#12013 = EDGE_CURVE ( 'NONE', #1879, #5410, #17147, .T. ) ;
#12014 = CARTESIAN_POINT ( 'NONE',  ( 6.484653179477954943, 49.78432281965648087, 78.61296362383696135 ) ) ;
#12015 = VERTEX_POINT ( 'NONE', #5965 ) ;
#12016 = CARTESIAN_POINT ( 'NONE',  ( 5.579938407236030073, 50.61660530761176346, 76.19612812024240611 ) ) ;
#12017 = CARTESIAN_POINT ( 'NONE',  ( 0.5221537403065091842, 44.16218137147969713, 58.55433879953100984 ) ) ;
#12018 = VECTOR ( 'NONE', #3899, 1000.000000000000227 ) ;
#12019 = CARTESIAN_POINT ( 'NONE',  ( 9.115819689944924420, 42.11441440976988559, 75.45386443748748206 ) ) ;
#12020 = CARTESIAN_POINT ( 'NONE',  ( 4.555266191169155654, 52.12349827269967761, 77.01204236660041147 ) ) ;
#12021 = CARTESIAN_POINT ( 'NONE',  ( -7.607912653626056176, 43.09321218401766629, 78.73993707373800532 ) ) ;
#12022 = CARTESIAN_POINT ( 'NONE',  ( -4.567115856812060670, 47.10047254335474065, 94.71121380123797451 ) ) ;
#12023 = CARTESIAN_POINT ( 'NONE',  ( 0.7555763647120519177, 52.35288517333821545, 77.43909148762901395 ) ) ;
#12024 = DIRECTION ( 'NONE',  ( -0.9534635866061452747, -0.3015081906286225522, -2.009271279954815797E-16 ) ) ;
#12025 = CARTESIAN_POINT ( 'NONE',  ( 4.097390034816025484, 51.53687999803451447, 76.58963291717793709 ) ) ;
#12026 = CARTESIAN_POINT ( 'NONE',  ( -2.904223097202481174, 48.62752260303690122, 94.08621380294496817 ) ) ;
#12027 = CARTESIAN_POINT ( 'NONE',  ( -7.373282680283180568, 41.96158783262483638, 78.50654468188380974 ) ) ;
#12028 = ORIENTED_EDGE ( 'NONE', *, *, #416, .F. ) ;
#12029 = CARTESIAN_POINT ( 'NONE',  ( -4.517072128342570991, 36.94403992325788977, 76.53375056423675460 ) ) ;
#12030 = AXIS2_PLACEMENT_3D ( 'NONE', #11882, #10624, #5589 ) ;
#12031 = ORIENTED_EDGE ( 'NONE', *, *, #15429, .F. ) ;
#12032 = CARTESIAN_POINT ( 'NONE',  ( -4.579686653871014812, 36.99029075099881680, 76.02016401025396419 ) ) ;
#12033 = DIRECTION ( 'NONE',  ( -1.402518428993830937E-16, 1.000000000000000000, -3.469446951953617147E-16 ) ) ;
#12034 = CARTESIAN_POINT ( 'NONE',  ( 5.327803506469481754, 40.48109702276099853, 75.45433879953087342 ) ) ;
#12035 = CARTESIAN_POINT ( 'NONE',  ( 6.198496396448986090, 45.68315280215533392, 92.99246380123798872 ) ) ;
#12036 = CARTESIAN_POINT ( 'NONE',  ( -4.871646723878168217, 37.20594989384409956, 76.06675994099744287 ) ) ;
#12037 = CARTESIAN_POINT ( 'NONE',  ( -1.477846259693495590, 47.62628298661744708, 61.15433879953099705 ) ) ;
#12038 = DIRECTION ( 'NONE',  ( -0.3165065846431827645, -0.9485903129789529098, 0.000000000000000000 ) ) ;
#12039 = VERTEX_POINT ( 'NONE', #12153 ) ;
#12040 = CARTESIAN_POINT ( 'NONE',  ( 9.244427017087200937, 42.49985872791199881, 79.25343573416346032 ) ) ;
#12041 = LINE ( 'NONE', #2239, #16902 ) ;
#12042 = DIRECTION ( 'NONE',  ( -0.8660254037844397068, -0.4999999999999981126, -0.000000000000000000 ) ) ;
#12043 = ORIENTED_EDGE ( 'NONE', *, *, #17712, .T. ) ;
#12044 = CARTESIAN_POINT ( 'NONE',  ( 5.770850603891227060, 51.22559503374887413, 77.28904345712264501 ) ) ;
#12045 = CARTESIAN_POINT ( 'NONE',  ( -3.105421771460856295, 39.66752508378051090, 95.05433879953098142 ) ) ;
#12046 = CARTESIAN_POINT ( 'NONE',  ( -1.187946976321871961, 48.86064447540922373, 92.79808879611698558 ) ) ;
#12047 = DIRECTION ( 'NONE',  ( 3.893792155548169402E-16, 7.183611964723547524E-17, -1.000000000000000000 ) ) ;
#12048 = CARTESIAN_POINT ( 'NONE',  ( 1.417490718652078652, 52.94576632079922263, 76.80858772049349170 ) ) ;
#12049 = CARTESIAN_POINT ( 'NONE',  ( 11.22215374030650281, 42.76218137147968434, 69.80574467885101342 ) ) ;
#12050 = CARTESIAN_POINT ( 'NONE',  ( -3.350035803220276609, 49.20851703305431357, 93.22683880123798872 ) ) ;
#12051 = CARTESIAN_POINT ( 'NONE',  ( -8.156636136238528678, 42.70560223241731990, 79.14287594667040082 ) ) ;
#12052 = ORIENTED_EDGE ( 'NONE', *, *, #1932, .T. ) ;
#12053 = CARTESIAN_POINT ( 'NONE',  ( 5.439084145646494228, 50.71602161008325282, 77.28794373216803137 ) ) ;
#12054 = VERTEX_POINT ( 'NONE', #762 ) ;
#12055 = DIRECTION ( 'NONE',  ( 0.3165065846431826535, 0.9485903129789529098, 2.188653791613874008E-16 ) ) ;
#12056 = CARTESIAN_POINT ( 'NONE',  ( 3.948530577815480225, 39.69684013992245752, 94.71121380294496817 ) ) ;
#12057 = ORIENTED_EDGE ( 'NONE', *, *, #16399, .T. ) ;
#12058 = CARTESIAN_POINT ( 'NONE',  ( 2.722153740306497927, 50.36218137147968577, 50.15433879953098995 ) ) ;
#12059 = CARTESIAN_POINT ( 'NONE',  ( -4.539611090124166637, 51.36100176422416297, 79.54777180229389444 ) ) ;
#12060 = DIRECTION ( 'NONE',  ( 1.000000000000000000, -0.000000000000000000, -0.000000000000000000 ) ) ;
#12061 = CARTESIAN_POINT ( 'NONE',  ( 0.3481951245351748159, 52.36035653588419336, 77.54150877948023890 ) ) ;
#12062 = CARTESIAN_POINT ( 'NONE',  ( 0.3607744984173847924, 52.35599833409515469, 78.79918605040184332 ) ) ;
#12063 = ORIENTED_EDGE ( 'NONE', *, *, #20431, .F. ) ;
#12064 = DIRECTION ( 'NONE',  ( 0.3165065846431828200, 0.9485903129789527988, 0.000000000000000000 ) ) ;
#12065 = ORIENTED_EDGE ( 'NONE', *, *, #19875, .T. ) ;
#12066 = CARTESIAN_POINT ( 'NONE',  ( 6.488291687484917247, 49.78758830262064095, 78.40346922251953288 ) ) ;
#12067 = CARTESIAN_POINT ( 'NONE',  ( 23.03948732994508575, 36.35905713404685002, 77.50433879953099847 ) ) ;
#12068 = DIRECTION ( 'NONE',  ( 0.8660254037844399289, 0.4999999999999977796, 0.000000000000000000 ) ) ;
#12069 = ADVANCED_FACE ( 'NONE', ( #2472 ), #18946, .F. ) ;
#12070 = CARTESIAN_POINT ( 'NONE',  ( -7.497325726272184632, 40.53822013297730820, 77.43474300570518665 ) ) ;
#12071 = CARTESIAN_POINT ( 'NONE',  ( 5.856396280011940014, 46.10368687828906076, 93.34496379782399345 ) ) ;
#12072 = DIRECTION ( 'NONE',  ( 4.818676322157797375E-16, 1.000000000000000000, -0.000000000000000000 ) ) ;
#12073 = ORIENTED_EDGE ( 'NONE', *, *, #6746, .F. ) ;
#12074 = CARTESIAN_POINT ( 'NONE',  ( 4.120959222841843683, 51.53026784114320691, 77.04928664276771144 ) ) ;
#12075 = ORIENTED_EDGE ( 'NONE', *, *, #11662, .T. ) ;
#12076 = CARTESIAN_POINT ( 'NONE',  ( -4.157721234522135489, 51.63388627315737267, 75.40660817806873695 ) ) ;
#12077 = EDGE_CURVE ( 'NONE', #18429, #4049, #2411, .T. ) ;
#12078 = CARTESIAN_POINT ( 'NONE',  ( 5.025485839985549319, 41.56218137147963887, 94.47683879953099506 ) ) ;
#12079 = CARTESIAN_POINT ( 'NONE',  ( -3.943187491250720544, 40.73580453397070755, 96.58621379953099506 ) ) ;
#12080 = VERTEX_POINT ( 'NONE', #4162 ) ;
#12081 = CARTESIAN_POINT ( 'NONE',  ( 4.394343283833276992, 39.11584570990505938, 94.00808880123797451 ) ) ;
#12082 = CARTESIAN_POINT ( 'NONE',  ( -5.784195910403845176, 44.99242805365518194, 94.63308880123808819 ) ) ;
#12083 = CARTESIAN_POINT ( 'NONE',  ( -3.602792415931784120, 40.47352456204527016, 95.05433879953102405 ) ) ;
#12084 = DIRECTION ( 'NONE',  ( 0.007885122365275663500, 0.9999689119394085113, 1.805443505845543142E-16 ) ) ;
#12085 = CARTESIAN_POINT ( 'NONE',  ( 1.256812508749381774, 49.74246873332880625, 92.36746379953098085 ) ) ;
#12086 = ADVANCED_FACE ( 'NONE', ( #10575 ), #15656, .T. ) ;
#12087 = ORIENTED_EDGE ( 'NONE', *, *, #19263, .T. ) ;
#12088 = CARTESIAN_POINT ( 'NONE',  ( 28.94982316289697621, 40.36218137147969287, 87.65433879953101837 ) ) ;
#12089 = CARTESIAN_POINT ( 'NONE',  ( -3.350035803220276609, 49.20851703305431357, 94.63308880123798872 ) ) ;
#12090 = ORIENTED_EDGE ( 'NONE', *, *, #19646, .T. ) ;
#12091 = CARTESIAN_POINT ( 'NONE',  ( 0.8440319792177738423, 52.35586314820839249, 77.67431863760063493 ) ) ;
#12092 = CARTESIAN_POINT ( 'NONE',  ( 5.190347370342537126, 37.42057832489953739, 75.99789977449030687 ) ) ;
#12093 = EDGE_CURVE ( 'NONE', #13846, #3162, #2774, .T. ) ;
#12094 = PLANE ( 'NONE',  #12030 ) ;
#12095 = EDGE_CURVE ( 'NONE', #15360, #20516, #12632, .T. ) ;
#12096 = CARTESIAN_POINT ( 'NONE',  ( -4.501113814897558463, 37.68688810195902050, 76.03818239474222196 ) ) ;
#12097 = CARTESIAN_POINT ( 'NONE',  ( 0.3326973149608338787, 52.96014171822455552, 78.50066232894263862 ) ) ;
#12098 = PLANE ( 'NONE',  #15720 ) ;
#12099 = EDGE_CURVE ( 'NONE', #4049, #4681, #16285, .T. ) ;
#12100 = EDGE_LOOP ( 'NONE', ( #10813, #20953, #19649, #15178 ) ) ;
#12101 = EDGE_LOOP ( 'NONE', ( #1350, #13179, #7302, #2965, #5585, #9399 ) ) ;
#12102 = ADVANCED_FACE ( 'NONE', ( #15973 ), #9802, .T. ) ;
#12103 = CARTESIAN_POINT ( 'NONE',  ( 2.114015745586784512, 52.20152540548682651, 76.39978148915828626 ) ) ;
#12104 = ORIENTED_EDGE ( 'NONE', *, *, #2826, .F. ) ;
#12105 = DIRECTION ( 'NONE',  ( 1.110223024625156540E-16, 1.000000000000000000, 5.922860397471808077E-17 ) ) ;
#12106 = CARTESIAN_POINT ( 'NONE',  ( 0.4760101966287402786, 52.96644344090527312, 77.40025757944940210 ) ) ;
#12107 = CARTESIAN_POINT ( 'NONE',  ( -4.567115856812060670, 47.10047254335474065, 94.71121380123797451 ) ) ;
#12108 = VERTEX_POINT ( 'NONE', #17555 ) ;
#12109 = LINE ( 'NONE', #15409, #5542 ) ;
#12110 = VERTEX_POINT ( 'NONE', #6171 ) ;
#12111 = CARTESIAN_POINT ( 'NONE',  ( -3.899663497332586104, 36.48798503826752437, 77.67016408458685817 ) ) ;
#12112 = LINE ( 'NONE', #20393, #5765 ) ;
#12113 = CARTESIAN_POINT ( 'NONE',  ( 31.03948732994507864, 45.16218137147969003, 76.90433879953100416 ) ) ;
#12114 = CARTESIAN_POINT ( 'NONE',  ( -7.324458055672637968, 41.78044449906338542, 78.92964119392561884 ) ) ;
#12115 = CARTESIAN_POINT ( 'NONE',  ( 2.522153740306505743, 50.16218137147969713, 82.55433879953099563 ) ) ;
#12116 = FACE_OUTER_BOUND ( 'NONE', #2963, .T. ) ;
#12117 = B_SPLINE_SURFACE_WITH_KNOTS ( 'NONE', 3, 1, ( 
 ( #17531, #9460 ),
 ( #15945, #7856 ),
 ( #10301, #16466 ),
 ( #1887, #19842 ),
 ( #6662, #13274 ),
 ( #2093, #1987 ),
 ( #8374, #13165 ),
 ( #19742, #10191 ),
 ( #16673, #5162 ),
 ( #19539, #16361 ),
 ( #8274, #18158 ),
 ( #488, #1791 ),
 ( #11886, #3578 ),
 ( #14963, #10083 ),
 ( #8594, #15074 ),
 ( #14757, #14649 ),
 ( #13065, #11474 ),
 ( #16565, #6868 ),
 ( #5081, #291 ),
 ( #6784, #13288 ),
 ( #19964, #8397 ),
 ( #298, #8082 ),
 ( #19152, #12278 ),
 ( #7876, #17866 ),
 ( #6265, #9795 ),
 ( #20731, #16074 ),
 ( #1497, #12869 ) ),
 .UNSPECIFIED., .F., .F., .F.,
 ( 4, 1, 1, 1, 1, 1, 1, 1, 1, 1, 1, 1, 1, 1, 1, 1, 1, 1, 1, 1, 1, 1, 1, 1, 4 ),
 ( 2, 2 ),
 ( 0.000000000000000000, 0.05959187408140657199, 0.1157444014141101180, 0.1691701821137891193, 0.2193251454534784761, 0.2669475916912845692, 0.3117751794269221777, 0.3541065092364359956, 0.3940487965473342680, 0.4318372767115636890, 0.4680493653760790518, 0.5025338411669280081, 0.5356117844586580912, 0.5674765898557931898, 0.5983444621881826020, 0.6284125990791417093, 0.6580179645932986432, 0.6886630208720043722, 0.7222707808379922323, 0.7592609375352028511, 0.7993858191113136780, 0.8438632570080943918, 0.8918964550480946718, 0.9439126001412549982, 1.000000000000000000 ),
 ( 0.000000000000000000, 1.000000000000000000 ),
 .UNSPECIFIED. ) ;
#12118 = CARTESIAN_POINT ( 'NONE',  ( 0.8299508218102534807, 52.96365248900040967, 77.55588632845071118 ) ) ;
#12119 = DIRECTION ( 'NONE',  ( -0.000000000000000000, -0.000000000000000000, -1.000000000000000000 ) ) ;
#12120 = CARTESIAN_POINT ( 'NONE',  ( -4.158578283022523969, 37.42937009194850617, 78.58080938776616620 ) ) ;
#12121 = EDGE_CURVE ( 'NONE', #8117, #19239, #20844, .T. ) ;
#12122 = CARTESIAN_POINT ( 'NONE',  ( 1.868012774839550749, 39.13936707477651566, 93.38308880294498238 ) ) ;
#12123 = CARTESIAN_POINT ( 'NONE',  ( 11.22215374030650281, 42.96218137147968008, 58.20715055817105110 ) ) ;
#12124 = ORIENTED_EDGE ( 'NONE', *, *, #12237, .T. ) ;
#12125 = ADVANCED_FACE ( 'NONE', ( #6373 ), #12773, .F. ) ;
#12126 = EDGE_CURVE ( 'NONE', #13051, #15145, #16417, .T. ) ;
#12127 = EDGE_CURVE ( 'NONE', #5907, #2608, #4685, .T. ) ;
#12128 = VECTOR ( 'NONE', #18155, 1000.000000000000000 ) ;
#12129 = ORIENTED_EDGE ( 'NONE', *, *, #6187, .F. ) ;
#12130 = DIRECTION ( 'NONE',  ( 0.3165065846431827645, 0.9485903129789529098, 0.000000000000000000 ) ) ;
#12131 = PLANE ( 'NONE',  #1763 ) ;
#12132 = CARTESIAN_POINT ( 'NONE',  ( 8.386782761808312614, 39.92944448690413140, 78.16120960217517677 ) ) ;
#12133 = CARTESIAN_POINT ( 'NONE',  ( 6.828503391016846891, 43.33193468930419101, 95.41433880123797451 ) ) ;
#12134 = CARTESIAN_POINT ( 'NONE',  ( -4.895069120933021267, 37.22325107503680641, 76.32271929704664615 ) ) ;
#12135 = CARTESIAN_POINT ( 'NONE',  ( -6.788816072239765020, 47.86659415929654671, 78.78375056423675460 ) ) ;
#12136 = CARTESIAN_POINT ( 'NONE',  ( -0.4699484075730042676, 52.36218137147968577, 52.53721119516358584 ) ) ;
#12137 = CARTESIAN_POINT ( 'NONE',  ( 5.894623494294806143, 51.13416898548390321, 78.12411320240556734 ) ) ;
#12138 = ORIENTED_EDGE ( 'NONE', *, *, #11484, .F. ) ;
#12139 = ORIENTED_EDGE ( 'NONE', *, *, #2826, .T. ) ;
#12140 = CARTESIAN_POINT ( 'NONE',  ( 8.467255801511027968, 42.53504534252056857, 79.38025142445083304 ) ) ;
#12141 = CARTESIAN_POINT ( 'NONE',  ( -6.753843712027886248, 40.38066566033639759, 72.45433879953085921 ) ) ;
#12142 = CARTESIAN_POINT ( 'NONE',  ( 4.470572738639666532, 36.16780480931087283, 79.45433879953087342 ) ) ;
#12143 = CARTESIAN_POINT ( 'NONE',  ( -1.477846259693493369, 50.16218137147969713, 77.15433879953100416 ) ) ;
#12144 = CARTESIAN_POINT ( 'NONE',  ( 5.562547263452509938, 51.37946032036057886, 77.00567114208729436 ) ) ;
#12145 = AXIS2_PLACEMENT_3D ( 'NONE', #6280, #14481, #14161 ) ;
#12146 = CARTESIAN_POINT ( 'NONE',  ( 8.316956916703102110, 42.08459004996775121, 78.13669174070733447 ) ) ;
#12147 = CARTESIAN_POINT ( 'NONE',  ( -3.943187491250720544, 40.73580453397070755, 90.64871380294496817 ) ) ;
#12148 = CARTESIAN_POINT ( 'NONE',  ( 0.1681371321675577124, 52.95815348057784888, 79.53018714708582593 ) ) ;
#12149 = CARTESIAN_POINT ( 'NONE',  ( -7.062866454872595234, 47.10224949948419493, 78.22140724958771330 ) ) ;
#12150 = EDGE_CURVE ( 'NONE', #18554, #6620, #2148, .T. ) ;
#12151 = CARTESIAN_POINT ( 'NONE',  ( 3.788215052820487205, 39.19523464621513398, 90.08681233796825438 ) ) ;
#12152 = ORIENTED_EDGE ( 'NONE', *, *, #19002, .F. ) ;
#12153 = CARTESIAN_POINT ( 'NONE',  ( 6.691294758883309157, 37.75465145915448062, 79.45433879953087342 ) ) ;
#12154 = ORIENTED_EDGE ( 'NONE', *, *, #6626, .F. ) ;
#12155 = VECTOR ( 'NONE', #5284, 1000.000000000000227 ) ;
#12156 = CARTESIAN_POINT ( 'NONE',  ( -4.451219113684727446, 50.67724800213075298, 78.47639829077699858 ) ) ;
#12157 = CARTESIAN_POINT ( 'NONE',  ( -4.524181921268124462, 40.28999182795290324, 92.28933880123798872 ) ) ;
#12158 =( BOUNDED_CURVE ( )  B_SPLINE_CURVE ( 2, ( #15355, #6932, #18641, #10370, #661, #10152, #2052, #2258, #13748, #2478, #3951 ),
 .UNSPECIFIED., .F., .F. ) 
 B_SPLINE_CURVE_WITH_KNOTS ( ( 3, 2, 2, 2, 2, 3 ),
 ( 0.7673390146554853741, 0.7812500000000000000, 0.8125000000000000000, 0.8437500000000000000, 0.8750000000000000000, 0.8923390146554854852 ),
 .UNSPECIFIED. ) 
 CURVE ( )  GEOMETRIC_REPRESENTATION_ITEM ( )  RATIONAL_B_SPLINE_CURVE ( ( 0.9623977609649205789, 0.9661148573551010532, 1.000000000000000000, 0.9238795325112867385, 1.000000000000000000, 0.9238795325112867385, 1.000000000000000000, 0.9238795325112867385, 1.000000000000000000, 0.9577646751561854632, 0.9623977609649205789 ) ) 
 REPRESENTATION_ITEM ( '' )  );
#12159 = EDGE_LOOP ( 'NONE', ( #6653, #16490, #18339, #4454, #5658, #5306, #20168, #9407 ) ) ;
#12160 = CARTESIAN_POINT ( 'NONE',  ( -3.950384684012687053, 48.00272989695906745, 92.51086634195935687 ) ) ;
#12161 = CARTESIAN_POINT ( 'NONE',  ( -3.491755833756905236, 51.18998518371629558, 79.42193487995672285 ) ) ;
#12162 = CARTESIAN_POINT ( 'NONE',  ( 0.8384463289470892589, 52.95649690220134431, 77.58758240811609141 ) ) ;
#12163 = CARTESIAN_POINT ( 'NONE',  ( -4.477846259693478714, 37.66295064777091994, 53.55433879953098852 ) ) ;
#12164 = CARTESIAN_POINT ( 'NONE',  ( -3.110947477468488209, 36.81940729104130128, 78.70659543854199569 ) ) ;
#12165 = ORIENTED_EDGE ( 'NONE', *, *, #8390, .T. ) ;
#12166 = FACE_OUTER_BOUND ( 'NONE', #11773, .T. ) ;
#12167 = AXIS2_PLACEMENT_3D ( 'NONE', #10981, #4459, #14142 ) ;
#12168 = ORIENTED_EDGE ( 'NONE', *, *, #16420, .F. ) ;
#12169 = EDGE_CURVE ( 'NONE', #10787, #13741, #6688, .T. ) ;
#12170 = CARTESIAN_POINT ( 'NONE',  ( 0.5221537403065040772, 39.16218137147969003, 94.91636871766883132 ) ) ;
#12171 = CARTESIAN_POINT ( 'NONE',  ( 11.22215374030649926, 42.76218137147968434, 80.55433879953099563 ) ) ;
#12172 = CARTESIAN_POINT ( 'NONE',  ( 0.5221537403065019678, 44.16218137147968292, 72.45433879953087342 ) ) ;
#12173 = CARTESIAN_POINT ( 'NONE',  ( -3.777846259693486974, 36.96218137147968008, 53.35433879953099989 ) ) ;
#12174 = CARTESIAN_POINT ( 'NONE',  ( 6.923174433796239313, 50.37441983903331533, 78.52964612251847143 ) ) ;
#12175 = CARTESIAN_POINT ( 'NONE',  ( -1.677846259693485109, 49.95873206995546667, 56.15433879953099705 ) ) ;
#12176 = CARTESIAN_POINT ( 'NONE',  ( -3.628867371436363953, 48.69222599884265179, 93.73558879782397923 ) ) ;
#12177 = CARTESIAN_POINT ( 'NONE',  ( 5.404201196092212278, 50.75047497752489534, 79.54845644658969661 ) ) ;
#12178 = ORIENTED_EDGE ( 'NONE', *, *, #16781, .T. ) ;
#12179 = CARTESIAN_POINT ( 'NONE',  ( 8.228415462672815650, 41.37506577911731398, 78.86399424569901839 ) ) ;
#12180 = AXIS2_PLACEMENT_3D ( 'NONE', #9698, #14675, #12980 ) ;
#12181 = ORIENTED_EDGE ( 'NONE', *, *, #14421, .T. ) ;
#12182 = CARTESIAN_POINT ( 'NONE',  ( -4.037464293073704802, 50.80004189835040762, 75.36471306604558151 ) ) ;
#12183 = CARTESIAN_POINT ( 'NONE',  ( 3.122153740306552905, 48.66551347115873227, 96.03933879953099506 ) ) ;
#12184 = EDGE_LOOP ( 'NONE', ( #17550, #5876, #19314 ) ) ;
#12185 = EDGE_CURVE ( 'NONE', #6294, #15169, #6691, .T. ) ;
#12186 = CARTESIAN_POINT ( 'NONE',  ( -3.350035803220276609, 49.20851703305431357, 92.13308880123798872 ) ) ;
#12187 = CARTESIAN_POINT ( 'NONE',  ( 4.470572738639666532, 36.16780480931087283, 79.45433879953087342 ) ) ;
#12188 = CARTESIAN_POINT ( 'NONE',  ( -6.792737292293178797, 47.86790251333490431, 78.32492703482499508 ) ) ;
#12189 = CARTESIAN_POINT ( 'NONE',  ( 6.880132251722071324, 48.33664052787082710, 72.45432679953087529 ) ) ;
#12190 = EDGE_LOOP ( 'NONE', ( #8467, #2500, #12075, #878 ) ) ;
#12191 = DIRECTION ( 'NONE',  ( 1.000000000000000000, 0.000000000000000000, 0.000000000000000000 ) ) ;
#12192 = CARTESIAN_POINT ( 'NONE',  ( -0.9988176903691428077, 49.83852402762217082, 93.30496380123798872 ) ) ;
#12193 = ORIENTED_EDGE ( 'NONE', *, *, #9750, .T. ) ;
#12194 = CARTESIAN_POINT ( 'NONE',  ( -4.309867278466398055, 50.78806163760442161, 79.54633918777975055 ) ) ;
#12195 = FACE_OUTER_BOUND ( 'NONE', #7796, .T. ) ;
#12196 = CARTESIAN_POINT ( 'NONE',  ( 9.176231272041631470, 45.98187388689780164, 75.44992703482499508 ) ) ;
#12197 = VECTOR ( 'NONE', #11008, 1000.000000000000000 ) ;
#12198 = DIRECTION ( 'NONE',  ( 0.000000000000000000, 0.000000000000000000, 1.000000000000000000 ) ) ;
#12199 = CARTESIAN_POINT ( 'NONE',  ( -4.517232838915925974, 37.69879457568749359, 76.09452555557021469 ) ) ;
#12200 = ADVANCED_FACE ( 'NONE', ( #11508 ), #7837, .F. ) ;
#12201 = CARTESIAN_POINT ( 'NONE',  ( 5.614631715549363022, 51.34098763368633911, 78.82175487302160377 ) ) ;
#12202 = CARTESIAN_POINT ( 'NONE',  ( -7.506717439198443920, 42.46581745002679753, 76.87606454720180693 ) ) ;
#12203 = VERTEX_POINT ( 'NONE', #18400 ) ;
#12204 = CARTESIAN_POINT ( 'NONE',  ( 1.637918093877997361, 52.95811772167194675, 75.56770918405875648 ) ) ;
#12205 = EDGE_LOOP ( 'NONE', ( #10766, #19310, #8356, #14833 ) ) ;
#12206 = CARTESIAN_POINT ( 'NONE',  ( -0.8970780467398890012, 52.23845657948073296, 78.77588839903116025 ) ) ;
#12207 = LINE ( 'NONE', #9126, #9586 ) ;
#12208 = CARTESIAN_POINT ( 'NONE',  ( 5.611423337425062385, 41.22389019960463230, 90.33621380123798872 ) ) ;
#12209 = CARTESIAN_POINT ( 'NONE',  ( -3.396200966244447450, 52.17804077583208766, 76.13050287850805375 ) ) ;
#12210 = ORIENTED_EDGE ( 'NONE', *, *, #15507, .T. ) ;
#12211 = AXIS2_PLACEMENT_3D ( 'NONE', #10153, #6516, #9946 ) ;
#12212 = FACE_OUTER_BOUND ( 'NONE', #10078, .T. ) ;
#12213 = ORIENTED_EDGE ( 'NONE', *, *, #12241, .F. ) ;
#12214 = CARTESIAN_POINT ( 'NONE',  ( 4.905034931190686009, 51.86513819399005598, 79.33697856897433098 ) ) ;
#12215 = DIRECTION ( 'NONE',  ( -1.402518428993830937E-16, 1.000000000000000000, -3.469446951953617147E-16 ) ) ;
#12216 = CARTESIAN_POINT ( 'NONE',  ( -4.884656273474450749, 44.39824779480852612, 92.09496379953097289 ) ) ;
#12217 = CARTESIAN_POINT ( 'NONE',  ( 5.451303755781102822, 37.60902651911217731, 77.68277620389109472 ) ) ;
#12218 = LINE ( 'NONE', #13705, #11821 ) ;
#12219 = FACE_OUTER_BOUND ( 'NONE', #13971, .T. ) ;
#12220 = LINE ( 'NONE', #9141, #15072 ) ;
#12221 = FACE_OUTER_BOUND ( 'NONE', #18564, .T. ) ;
#12222 = AXIS2_PLACEMENT_3D ( 'NONE', #20883, #12719, #11551 ) ;
#12223 = LINE ( 'NONE', #14514, #17654 ) ;
#12224 = CARTESIAN_POINT ( 'NONE',  ( 5.722153871292735339, 42.76884579771262906, 94.83987682607160252 ) ) ;
#12225 = EDGE_CURVE ( 'NONE', #4837, #140, #1822, .T. ) ;
#12226 = CARTESIAN_POINT ( 'NONE',  ( 5.544968037009670780, 45.50804040601273925, 91.19558880294498238 ) ) ;
#12227 = AXIS2_PLACEMENT_3D ( 'NONE', #1060, #7435, #4232 ) ;
#12228 = CARTESIAN_POINT ( 'NONE',  ( 2.263363662449358493, 49.77488197367694767, 94.44231768333818877 ) ) ;
#12229 = CARTESIAN_POINT ( 'NONE',  ( 8.941920682866751235, 41.59322805360929465, 78.83412695248559032 ) ) ;
#12230 = AXIS2_PLACEMENT_3D ( 'NONE', #12017, #4112, #2313 ) ;
#12231 = ORIENTED_EDGE ( 'NONE', *, *, #17431, .T. ) ;
#12232 = LINE ( 'NONE', #9363, #4400 ) ;
#12233 = AXIS2_PLACEMENT_3D ( 'NONE', #14928, #6940, #13346 ) ;
#12234 = CARTESIAN_POINT ( 'NONE',  ( 0.5221537403065019678, 44.16218137147968292, 72.45433879953087342 ) ) ;
#12235 = CARTESIAN_POINT ( 'NONE',  ( -3.512376142844359173, 52.09502624807847582, 79.07098488719154261 ) ) ;
#12236 = CARTESIAN_POINT ( 'NONE',  ( 6.198496396448986090, 45.68315280215533392, 94.24246380123798872 ) ) ;
#12237 = EDGE_CURVE ( 'NONE', #2058, #5122, #5947, .T. ) ;
#12238 = CARTESIAN_POINT ( 'NONE',  ( -4.883901707777988932, 37.21500215679002821, 76.12782976279942204 ) ) ;
#12239 = CARTESIAN_POINT ( 'NONE',  ( -7.195832550073633094, 46.64673995458454669, 79.32924967153994089 ) ) ;
#12240 = CARTESIAN_POINT ( 'NONE',  ( 5.631785411401764918, 36.99756487055721976, 77.76022115247205591 ) ) ;
#12241 = EDGE_CURVE ( 'NONE', #585, #19492, #8406, .T. ) ;
#12242 = CARTESIAN_POINT ( 'NONE',  ( -5.661408436751226070, 39.74363423441516829, 72.45432679953087529 ) ) ;
#12243 = AXIS2_PLACEMENT_3D ( 'NONE', #19322, #14340, #14545 ) ;
#12244 = ORIENTED_EDGE ( 'NONE', *, *, #768, .T. ) ;
#12245 = VERTEX_POINT ( 'NONE', #5299 ) ;
#12246 = VECTOR ( 'NONE', #17820, 1000.000000000000000 ) ;
#12247 = CARTESIAN_POINT ( 'NONE',  ( 8.608186895778700887, 42.95742477254270852, 78.97126489842982267 ) ) ;
#12248 = CARTESIAN_POINT ( 'NONE',  ( -4.320790804570143528, 36.79905481608121676, 75.39293290059653430 ) ) ;
#12249 = EDGE_CURVE ( 'NONE', #7189, #14664, #11813, .T. ) ;
#12250 = CARTESIAN_POINT ( 'NONE',  ( 8.949991632966883159, 41.61741720307092152, 76.25788209700408515 ) ) ;
#12252 = EDGE_CURVE ( 'NONE', #10416, #2282, #18442, .T. ) ;
#12251 = CARTESIAN_POINT ( 'NONE',  ( 5.916041096196198446, 51.11834866571297908, 77.16780247135808679 ) ) ;
#12253 = B_SPLINE_SURFACE_WITH_KNOTS ( 'NONE', 3, 1, ( 
 ( #11366, #14220 ),
 ( #6137, #12640 ),
 ( #19122, #9561 ),
 ( #3164, #12837 ),
 ( #12527, #4631 ),
 ( #1246, #21004 ),
 ( #19316, #9450 ),
 ( #11152, #7739 ),
 ( #6439, #15936 ),
 ( #4732, #9666 ),
 ( #12948, #19428 ) ),
 .UNSPECIFIED., .F., .F., .F.,
 ( 4, 1, 1, 1, 1, 1, 1, 1, 4 ),
 ( 2, 2 ),
 ( 0.000000000000000000, 0.1182921183292337947, 0.2229146666077276573, 0.3191072744444787279, 0.4123240778398947204, 0.5160602913484956256, 0.6446607815519475038, 0.8056994663548258107, 1.000000000000000000 ),
 ( 0.000000000000000000, 1.000000000000000000 ),
 .UNSPECIFIED. ) ;
#12254 = DIRECTION ( 'NONE',  ( -0.9534635866061452747, -0.3015081906286225522, -2.009271279954815797E-16 ) ) ;
#12255 = AXIS2_PLACEMENT_3D ( 'NONE', #10376, #16846, #2265 ) ;
#12256 = CARTESIAN_POINT ( 'NONE',  ( 8.396447191880023198, 42.32282744744201608, 78.11626675975762168 ) ) ;
#12257 = CARTESIAN_POINT ( 'NONE',  ( 5.544968037009670780, 45.50804040601273925, 93.69558880294498238 ) ) ;
#12258 = CARTESIAN_POINT ( 'NONE',  ( -4.592862224480081856, 51.32295045326188898, 75.97198585835440099 ) ) ;
#12259 = CARTESIAN_POINT ( 'NONE',  ( -7.088565933990943257, 47.02522653022194987, 77.78596583901244799 ) ) ;
#12260 = CARTESIAN_POINT ( 'NONE',  ( -5.784195910403845176, 44.99242805365518194, 90.88308880123798872 ) ) ;
#12261 = VECTOR ( 'NONE', #14029, 1000.000000000000000 ) ;
#12262 = CARTESIAN_POINT ( 'NONE',  ( 6.386300776676741897, 37.53671392601205525, 75.49608936836499140 ) ) ;
#12263 = EDGE_LOOP ( 'NONE', ( #13449, #11491, #18488, #12210 ) ) ;
#12264 = CARTESIAN_POINT ( 'NONE',  ( 2.115041367457930033, 52.20598078514408513, 76.48963291717792856 ) ) ;
#12265 = ORIENTED_EDGE ( 'NONE', *, *, #3514, .F. ) ;
#12266 = VECTOR ( 'NONE', #20543, 1000.000000000000000 ) ;
#12267 = CARTESIAN_POINT ( 'NONE',  ( -4.744888236371026302, 51.21431823119217341, 78.89490084226201816 ) ) ;
#12268 = CARTESIAN_POINT ( 'NONE',  ( -5.058133621542618030, 44.89684013992257405, 95.49246380294496817 ) ) ;
#12269 = ORIENTED_EDGE ( 'NONE', *, *, #10462, .T. ) ;
#12270 = CARTESIAN_POINT ( 'NONE',  ( -4.812088799398939187, 42.22067586467031930, 92.71996379782397923 ) ) ;
#12271 = CARTESIAN_POINT ( 'NONE',  ( -5.004817973257478236, 39.29348442311233214, 78.18375056423674607 ) ) ;
#12272 = CARTESIAN_POINT ( 'NONE',  ( -3.077292339936458454, 51.48614562192336308, 79.07098488719154261 ) ) ;
#12273 = CARTESIAN_POINT ( 'NONE',  ( 1.215246153217546921, 50.28109722957945138, 75.67325465763076409 ) ) ;
#12274 = PLANE ( 'NONE',  #20273 ) ;
#12275 = ADVANCED_FACE ( 'NONE', ( #15326 ), #8938, .T. ) ;
#12276 = FACE_OUTER_BOUND ( 'NONE', #8673, .T. ) ;
#12277 = ORIENTED_EDGE ( 'NONE', *, *, #10030, .F. ) ;
#12278 = CARTESIAN_POINT ( 'NONE',  ( 6.504942014150000951, 49.75851833300988858, 76.28194508213313441 ) ) ;
#12279 = DIRECTION ( 'NONE',  ( -1.540237394707283727E-16, -1.793354297423763257E-16, 1.000000000000000000 ) ) ;
#12280 = CARTESIAN_POINT ( 'NONE',  ( 4.673174852049362116, 39.63213674411673537, 92.95433879782399345 ) ) ;
#12281 = ORIENTED_EDGE ( 'NONE', *, *, #1014, .F. ) ;
#12282 = CARTESIAN_POINT ( 'NONE',  ( 2.232254456934870568, 39.46371826755015633, 94.98558879953097289 ) ) ;
#12283 = CARTESIAN_POINT ( 'NONE',  ( -4.517072128342571880, 36.94403992325788977, 78.34992703482498655 ) ) ;
#12284 = DIRECTION ( 'NONE',  ( 0.003108166696664913138, -0.009828999206266906055, -0.9999468636254573717 ) ) ;
#12285 = CARTESIAN_POINT ( 'NONE',  ( -0.9436870690626146807, 52.23009998296728895, 77.77566232894263010 ) ) ;
#12286 = CARTESIAN_POINT ( 'NONE',  ( -7.302117543854899750, 40.13466614431609258, 78.26848339007013067 ) ) ;
#12287 = DIRECTION ( 'NONE',  ( -0.9485903129789527988, 0.3165065846431829311, -8.934458285744989980E-17 ) ) ;
#12288 = CARTESIAN_POINT ( 'NONE',  ( -5.616286711741430793, 44.43019146960381960, 95.14183879782397923 ) ) ;
#12289 = CARTESIAN_POINT ( 'NONE',  ( 6.055018060417216574, 50.21607566361303299, 79.42942117149121373 ) ) ;
#12290 = EDGE_LOOP ( 'NONE', ( #20655, #13363, #6781, #14097 ) ) ;
#12291 = CARTESIAN_POINT ( 'NONE',  ( 4.527140486693829402, 51.31778872522085777, 77.65249324435147571 ) ) ;
#12292 = AXIS2_PLACEMENT_3D ( 'NONE', #12565, #20843, #6270 ) ;
#12293 =( BOUNDED_CURVE ( )  B_SPLINE_CURVE ( 2, ( #17636, #7653, #2762, #15531, #20615 ),
 .UNSPECIFIED., .F., .T. ) 
 B_SPLINE_CURVE_WITH_KNOTS ( ( 3, 2, 3 ),
 ( 0.5083811345117428271, 0.5250000000000000222, 0.5333811345117427383 ),
 .UNSPECIFIED. ) 
 CURVE ( )  GEOMETRIC_REPRESENTATION_ITEM ( )  RATIONAL_B_SPLINE_CURVE ( ( 0.9660722070828657859, 0.9493985675960727733, 1.000000000000000000, 0.9744809649152141873, 0.9660722070828660080 ) ) 
 REPRESENTATION_ITEM ( '' )  );
#12294 = EDGE_LOOP ( 'NONE', ( #9554, #16946, #14113, #10483 ) ) ;
#12295 = CARTESIAN_POINT ( 'NONE',  ( -4.621776214648809500, 51.30228957449607208, 75.36056307228784590 ) ) ;
#12296 = CARTESIAN_POINT ( 'NONE',  ( -0.2125050281363792815, 38.58189400963055959, 91.74246379953099506 ) ) ;
#12297 = CARTESIAN_POINT ( 'NONE',  ( -7.955322860971263843, 41.76477423154450008, 77.57193099691271243 ) ) ;
#12298 = EDGE_LOOP ( 'NONE', ( #1249, #8232, #16519, #4309, #6636 ) ) ;
#12299 = CARTESIAN_POINT ( 'NONE',  ( -0.9988176903691428077, 49.83852402762217082, 92.05496380123798872 ) ) ;
#12300 = CARTESIAN_POINT ( 'NONE',  ( -0.3080929418689875576, 37.85583172076932357, 94.94558880123805977 ) ) ;
#12301 = CARTESIAN_POINT ( 'NONE',  ( -1.582249008360334885, 39.19284116845371813, 95.05433879953098142 ) ) ;
#12302 = DIRECTION ( 'NONE',  ( -0.000000000000000000, -0.000000000000000000, 1.000000000000000000 ) ) ;
#12303 = ORIENTED_EDGE ( 'NONE', *, *, #5839, .F. ) ;
#12304 = CARTESIAN_POINT ( 'NONE',  ( 28.52215374030649642, 40.36218137147969287, 87.65433879953101837 ) ) ;
#12305 = CARTESIAN_POINT ( 'NONE',  ( 0.6748029067580463281, 52.96487981809853096, 78.92081865479288183 ) ) ;
#12306 = VECTOR ( 'NONE', #18614, 1000.000000000000114 ) ;
#12307 = VERTEX_POINT ( 'NONE', #15213 ) ;
#12308 = CARTESIAN_POINT ( 'NONE',  ( -5.073584210444301412, 50.15674762947981691, 79.28952735418165787 ) ) ;
#12309 = CARTESIAN_POINT ( 'NONE',  ( 10.77494014480653917, 42.76218137147968434, 58.20715055817105110 ) ) ;
#12310 = VECTOR ( 'NONE', #17537, 1000.000000000000114 ) ;
#12311 = APPLICATION_PROTOCOL_DEFINITION ( 'draft international standard', 'automotive_design', 1998, #9148 ) ;
#12312 = CARTESIAN_POINT ( 'NONE',  ( -3.899559394394517486, 36.48790814162070006, 77.72081520951157074 ) ) ;
#12313 = CARTESIAN_POINT ( 'NONE',  ( 5.753005855668248181, 51.23877623043087937, 78.93669174070734584 ) ) ;
#12314 = EDGE_CURVE ( 'NONE', #20066, #10307, #10662, .T. ) ;
#12315 = DIRECTION ( 'NONE',  ( -0.000000000000000000, 2.168404344970984413E-15, -1.000000000000000000 ) ) ;
#12316 = ORIENTED_EDGE ( 'NONE', *, *, #20131, .F. ) ;
#12317 = CARTESIAN_POINT ( 'NONE',  ( 1.193698689701933713, 52.96162055492719389, 75.41083127720757773 ) ) ;
#12318 = ORIENTED_EDGE ( 'NONE', *, *, #6498, .F. ) ;
#12319 = VECTOR ( 'NONE', #18282, 1000.000000000000000 ) ;
#12320 = DIRECTION ( 'NONE',  ( -0.000000000000000000, -0.000000000000000000, 1.000000000000000000 ) ) ;
#12321 = FACE_OUTER_BOUND ( 'NONE', #14766, .T. ) ;
#12322 = CARTESIAN_POINT ( 'NONE',  ( -0.9988176903691428077, 49.83852402762217082, 90.80496380123797451 ) ) ;
#12323 = VECTOR ( 'NONE', #16922, 1000.000000000000000 ) ;
#12324 = ORIENTED_EDGE ( 'NONE', *, *, #16156, .F. ) ;
#12325 = DIRECTION ( 'NONE',  ( 0.000000000000000000, -2.168404344970984413E-15, -1.000000000000000000 ) ) ;
#12326 = ORIENTED_EDGE ( 'NONE', *, *, #1693, .F. ) ;
#12327 = CARTESIAN_POINT ( 'NONE',  ( 5.166781194794222820, 50.75778176762062799, 79.54621928524807117 ) ) ;
#12328 = LINE ( 'NONE', #5608, #9169 ) ;
#12329 = CARTESIAN_POINT ( 'NONE',  ( 4.178421596892071932, 40.17206517740157778, 91.31371379953098710 ) ) ;
#12330 = CARTESIAN_POINT ( 'NONE',  ( -4.517387068041351483, 36.94427255652684039, 78.31852111096432623 ) ) ;
#12331 = CARTESIAN_POINT ( 'NONE',  ( -7.426618516485039123, 40.09345743339805068, 78.72343487459158951 ) ) ;
#12332 = CARTESIAN_POINT ( 'NONE',  ( -7.366006458923896716, 41.92050534979284038, 79.54485830165070581 ) ) ;
#12333 = LINE ( 'NONE', #4012, #11697 ) ;
#12334 = DIRECTION ( 'NONE',  ( 0.5941461771851692664, 0.8043570849667761591, 2.357623395011396791E-16 ) ) ;
#12336 = CARTESIAN_POINT ( 'NONE',  ( -5.403345028831681773, 49.82403353266325041, 76.76022115247205591 ) ) ;
#12335 = VECTOR ( 'NONE', #693, 1000.000000000000114 ) ;
#12337 = CARTESIAN_POINT ( 'NONE',  ( 4.891544444475510289, 50.95027012611001993, 75.39573407869305299 ) ) ;
#12338 = EDGE_CURVE ( 'NONE', #10285, #11136, #2650, .T. ) ;
#12339 = CARTESIAN_POINT ( 'NONE',  ( -2.077846259693550746, 39.65884927180063357, 90.72683880294498238 ) ) ;
#12340 = CIRCLE ( 'NONE', #11653, 0.5999999999999928724 ) ;
#12341 = EDGE_CURVE ( 'NONE', #14974, #6003, #16618, .T. ) ;
#12342 = CARTESIAN_POINT ( 'NONE',  ( -7.337607140633251923, 40.20406537192692298, 78.93275508898662451 ) ) ;
#12343 = CARTESIAN_POINT ( 'NONE',  ( 8.385679600361122255, 39.92613824206362949, 77.69330938776616335 ) ) ;
#12344 = CARTESIAN_POINT ( 'NONE',  ( -1.214884381343054987, 47.76843358786783256, 77.41730067788147096 ) ) ;
#12345 = DIRECTION ( 'NONE',  ( -1.000000000000000000, 1.193617070626243484E-16, 0.000000000000000000 ) ) ;
#12346 = CARTESIAN_POINT ( 'NONE',  ( -4.428870440144692999, 50.69880833818904620, 78.82590693216131683 ) ) ;
#12347 = CARTESIAN_POINT ( 'NONE',  ( 5.568489401881125289, 48.03437091500646261, 91.82058880123797451 ) ) ;
#12348 = VECTOR ( 'NONE', #6828, 1000.000000000000227 ) ;
#12349 = CARTESIAN_POINT ( 'NONE',  ( -0.3080929418689875576, 37.85583172076932357, 93.85183880123800293 ) ) ;
#12350 = CARTESIAN_POINT ( 'NONE',  ( -7.708574807372626125, 47.31288976295603277, 79.02985774836469091 ) ) ;
#12351 = CARTESIAN_POINT ( 'NONE',  ( 5.619997200715287633, 36.98914144679460492, 77.75986257808632729 ) ) ;
#12352 = EDGE_CURVE ( 'NONE', #18958, #7336, #7437, .T. ) ;
#12353 = EDGE_CURVE ( 'NONE', #9638, #5209, #9771, .T. ) ;
#12354 = CARTESIAN_POINT ( 'NONE',  ( 8.296628936784257391, 41.55497301399228149, 78.93669174070734584 ) ) ;
#12355 = CARTESIAN_POINT ( 'NONE',  ( -4.244029479098209379, 50.83477438462418974, 75.97198585835440099 ) ) ;
#12356 = DIRECTION ( 'NONE',  ( 0.5773502691896259531, 0.5773502691896257311, -0.5773502691896256200 ) ) ;
#12357 = CARTESIAN_POINT ( 'NONE',  ( -1.477846259693490705, 50.16218137147969713, 58.55433879953100984 ) ) ;
#12358 = CARTESIAN_POINT ( 'NONE',  ( -2.073200253767597090, 36.38374080505226971, 72.45433879953087342 ) ) ;
#12359 = DIRECTION ( 'NONE',  ( 1.779391786395883536E-16, 5.922860397471805611E-17, -1.000000000000000000 ) ) ;
#12360 = LINE ( 'NONE', #18838, #608 ) ;
#12361 = EDGE_CURVE ( 'NONE', #4917, #10614, #4910, .T. ) ;
#12362 = EDGE_CURVE ( 'NONE', #11879, #10061, #12546, .T. ) ;
#12363 = EDGE_CURVE ( 'NONE', #5674, #9005, #2901, .T. ) ;
#12364 = CARTESIAN_POINT ( 'NONE',  ( -0.9376789570059210766, 52.84025085569253122, 78.01128938824629699 ) ) ;
#12365 = CARTESIAN_POINT ( 'NONE',  ( -6.937748720045943784, 47.47723528808076310, 78.31886496287775401 ) ) ;
#12366 = DIRECTION ( 'NONE',  ( 1.540237394707284220E-16, 1.793354297423764243E-16, -1.000000000000000000 ) ) ;
#12367 = DIRECTION ( 'NONE',  ( -1.402518428993831676E-16, 1.000000000000000000, -0.000000000000000000 ) ) ;
#12368 = ORIENTED_EDGE ( 'NONE', *, *, #19872, .T. ) ;
#12369 = EDGE_CURVE ( 'NONE', #19774, #10630, #4450, .T. ) ;
#12370 = CARTESIAN_POINT ( 'NONE',  ( 5.939883047636084434, 51.10073757659671401, 76.92469047792664583 ) ) ;
#12371 = ORIENTED_EDGE ( 'NONE', *, *, #16723, .T. ) ;
#12372 = LINE ( 'NONE', #20000, #16985 ) ;
#12373 = CARTESIAN_POINT ( 'NONE',  ( 3.948530577815480225, 39.69684013992245752, 93.46121380294496817 ) ) ;
#12374 = ORIENTED_EDGE ( 'NONE', *, *, #13471, .F. ) ;
#12375 = CARTESIAN_POINT ( 'NONE',  ( -2.627048034785010699, 48.88511640015991588, 92.45433879952862810 ) ) ;
#12376 = CIRCLE ( 'NONE', #3863, 8.800000000000000711 ) ;
#12377 = CARTESIAN_POINT ( 'NONE',  ( -0.8532138448282817755, 52.21879250163868846, 76.01337353251631157 ) ) ;
#12378 = DIRECTION ( 'NONE',  ( 1.000000000000000000, -9.149887137874721638E-17, -0.000000000000000000 ) ) ;
#12379 = FACE_OUTER_BOUND ( 'NONE', #19039, .T. ) ;
#12380 = DIRECTION ( 'NONE',  ( -0.3165065846431825980, -0.9485903129789527988, 0.000000000000000000 ) ) ;
#12381 = CARTESIAN_POINT ( 'NONE',  ( -3.681032862722698695, 36.32649139546035855, 79.10742496273583413 ) ) ;
#12382 = VERTEX_POINT ( 'NONE', #11069 ) ;
#12383 = CARTESIAN_POINT ( 'NONE',  ( 8.305956354856951052, 41.60725829672735898, 75.97389479739716478 ) ) ;
#12384 = ORIENTED_EDGE ( 'NONE', *, *, #14662, .F. ) ;
#12385 = CARTESIAN_POINT ( 'NONE',  ( -3.055718635266669647, 36.78391400955043622, 76.62933879953087057 ) ) ;
#12386 = CARTESIAN_POINT ( 'NONE',  ( 3.961507247562194411, 36.71833509068318335, 72.45433879953087342 ) ) ;
#12387 = CARTESIAN_POINT ( 'NONE',  ( 13.32277635493562684, 36.96218137147968008, 80.55433879953099563 ) ) ;
#12388 = LINE ( 'NONE', #17066, #12197 ) ;
#12389 = CARTESIAN_POINT ( 'NONE',  ( -4.007890887056452911, 40.01116025973682611, 95.29808879782397923 ) ) ;
#12390 = ADVANCED_FACE ( 'NONE', ( #17538 ), #7863, .F. ) ;
#12391 = CARTESIAN_POINT ( 'NONE',  ( -6.374721436948748376, 46.24015083227975964, 79.45433879953087342 ) ) ;
#12392 = EDGE_LOOP ( 'NONE', ( #3754, #17521, #20199, #9443 ) ) ;
#12393 = EDGE_CURVE ( 'NONE', #15079, #3682, #3903, .T. ) ;
#12394 = CARTESIAN_POINT ( 'NONE',  ( 8.211300288254456348, 41.32377051561905290, 78.45948585835439815 ) ) ;
#12395 = ADVANCED_FACE ( 'NONE', ( #8067, #21023 ), #12963, .F. ) ;
#12396 = EDGE_LOOP ( 'NONE', ( #182, #6291, #3023, #2812 ) ) ;
#12397 = PLANE ( 'NONE',  #4418 ) ;
#12398 = CARTESIAN_POINT ( 'NONE',  ( 1.352400422481993658, 50.46853102219002096, 95.72683880123798872 ) ) ;
#12399 = CARTESIAN_POINT ( 'NONE',  ( 4.881482038019723468, 51.88253576740703465, 75.58280986828056314 ) ) ;
#12400 = ORIENTED_EDGE ( 'NONE', *, *, #19903, .T. ) ;
#12401 = CARTESIAN_POINT ( 'NONE',  ( 5.568489401881125289, 48.03437091500646261, 95.57058880123798872 ) ) ;
#12402 = CARTESIAN_POINT ( 'NONE',  ( -4.139151435122498945, 50.72720857236262759, 79.54845644658969661 ) ) ;
#12403 = ORIENTED_EDGE ( 'NONE', *, *, #7560, .F. ) ;
#12404 = CARTESIAN_POINT ( 'NONE',  ( 4.884665026186969961, 36.46369999710588417, 75.53067132529541539 ) ) ;
#12405 = CARTESIAN_POINT ( 'NONE',  ( -4.802657821332910082, 51.17303820085790278, 78.59458524649963351 ) ) ;
#12406 = ADVANCED_FACE ( 'NONE', ( #10203 ), #8382, .T. ) ;
#12407 = ORIENTED_EDGE ( 'NONE', *, *, #2758, .T. ) ;
#12408 = CARTESIAN_POINT ( 'NONE',  ( 1.602182432222049702, 52.29126342916185166, 79.36024077264127641 ) ) ;
#12409 = CARTESIAN_POINT ( 'NONE',  ( 2.043125170982144745, 38.48583871533720213, 92.67996380123798872 ) ) ;
#12410 = EDGE_LOOP ( 'NONE', ( #20807, #12441, #850, #11470 ) ) ;
#12411 = CARTESIAN_POINT ( 'NONE',  ( -5.405834154369066447, 49.82777573959609185, 78.20908272895746904 ) ) ;
#12412 = CARTESIAN_POINT ( 'NONE',  ( 31.22215374030650281, 45.56218137147968861, 78.80433879953099563 ) ) ;
#12413 = CARTESIAN_POINT ( 'NONE',  ( -5.616286711741430793, 44.43019146960381960, 93.89183879782397923 ) ) ;
#12414 = ITEM_DEFINED_TRANSFORMATION ( 'NONE', 'NONE', #13611,  #18366 ) ;
#12415 = CARTESIAN_POINT ( 'NONE',  ( 5.521494261397323022, 36.91875485278077207, 76.01263398532663018 ) ) ;
#12416 = CARTESIAN_POINT ( 'NONE',  ( 5.581823371501742237, 36.96186382607169207, 75.98067903659783440 ) ) ;
#12417 = CARTESIAN_POINT ( 'NONE',  ( 30.92220646078100188, 45.56218137147968861, 62.80715055817104542 ) ) ;
#12418 = ORIENTED_EDGE ( 'NONE', *, *, #13422, .F. ) ;
#12419 = CARTESIAN_POINT ( 'NONE',  ( 0.9669959323506999160, 52.21057007825091745, 75.37848164766056414 ) ) ;
#12420 = ORIENTED_EDGE ( 'NONE', *, *, #3216, .F. ) ;
#12421 = CARTESIAN_POINT ( 'NONE',  ( 0.5221537403065008576, 44.16218137147968292, 80.45433879953087342 ) ) ;
#12422 = CARTESIAN_POINT ( 'NONE',  ( 0.3528405447447653387, 52.36129150091981899, 75.36602869171218799 ) ) ;
#12423 = CARTESIAN_POINT ( 'NONE',  ( -0.3080929418689875576, 37.85583172076933778, 92.60183880123797451 ) ) ;
#12424 = B_SPLINE_SURFACE_WITH_KNOTS ( 'NONE', 3, 1, ( 
 ( #7890, #20851 ),
 ( #6279, #12780 ),
 ( #20446, #19261 ),
 ( #4675, #9604 ),
 ( #18853, #13314 ),
 ( #11724, #9809 ),
 ( #17779, #3206 ),
 ( #6380, #5205 ),
 ( #11622, #19572 ),
 ( #9921, #4781 ),
 ( #19471, #6699 ),
 ( #18196, #8415 ),
 ( #12885, #3302 ),
 ( #9708, #16187 ),
 ( #1613, #14892 ),
 ( #8204, #18096 ),
 ( #3518, #3411 ),
 ( #13203, #8097 ),
 ( #315, #16293 ) ),
 .UNSPECIFIED., .F., .F., .F.,
 ( 4, 1, 1, 1, 1, 1, 1, 1, 1, 1, 1, 1, 1, 1, 1, 1, 4 ),
 ( 2, 2 ),
 ( 0.000000000000000000, 0.07116601901339190961, 0.1384582187113551910, 0.2014355002094309066, 0.2607329607935783833, 0.3172301401005571675, 0.3704881719161017273, 0.4221645193212664182, 0.4717967126376631515, 0.5218096718684601676, 0.5745631757277218643, 0.6310618342314253670, 0.6925022631777019155, 0.7595319055140381526, 0.8328598856178031085, 0.9128843800434378597, 0.9999999999999998890 ),
 ( 0.000000000000000000, 1.000000000000000000 ),
 .UNSPECIFIED. ) ;
#12425 = EDGE_LOOP ( 'NONE', ( #16062, #3014, #10019, #10742, #5598 ) ) ;
#12426 = CARTESIAN_POINT ( 'NONE',  ( 0.5221537403065020788, 52.36218137147968577, 52.53721119516358584 ) ) ;
#12427 = ORIENTED_EDGE ( 'NONE', *, *, #14164, .F. ) ;
#12428 = CARTESIAN_POINT ( 'NONE',  ( 4.283022132325689846, 51.41057898707959595, 79.11209812681292419 ) ) ;
#12429 = DIRECTION ( 'NONE',  ( 1.540237394707284220E-16, 1.793354297423764243E-16, -1.000000000000000000 ) ) ;
#12430 = CARTESIAN_POINT ( 'NONE',  ( 7.680282685949594068, 40.19320369954859729, 76.21925085218815354 ) ) ;
#12431 = ORIENTED_EDGE ( 'NONE', *, *, #4099, .F. ) ;
#12432 = CARTESIAN_POINT ( 'NONE',  ( -7.677846259693483333, 47.36218137147966445, 95.05433879953098142 ) ) ;
#12433 = CARTESIAN_POINT ( 'NONE',  ( -6.891583108293479754, 40.88741496916635754, 79.38495514127318131 ) ) ;
#12434 = DIRECTION ( 'NONE',  ( 0.4999999999999977240, -0.8660254037844398178, 0.000000000000000000 ) ) ;
#12435 = CARTESIAN_POINT ( 'NONE',  ( 6.198496396448986090, 45.68315280215533392, 92.99246380123798872 ) ) ;
#12436 = DIRECTION ( 'NONE',  ( -0.5941461771851693774, -0.8043570849667760481, -2.357623395011396791E-16 ) ) ;
#12437 = CARTESIAN_POINT ( 'NONE',  ( 4.776132423410367700, 51.96035328397762498, 75.67068799376596644 ) ) ;
#12438 = EDGE_CURVE ( 'NONE', #1479, #14315, #1801, .T. ) ;
#12439 = CARTESIAN_POINT ( 'NONE',  ( 5.544968037009670780, 45.50804040601273925, 94.94558880294498238 ) ) ;
#12440 = CARTESIAN_POINT ( 'NONE',  ( 28.52215374030649642, 48.16218137147969003, 87.85433879953103542 ) ) ;
#12441 = ORIENTED_EDGE ( 'NONE', *, *, #6899, .T. ) ;
#12442 = CARTESIAN_POINT ( 'NONE',  ( 5.544968037009670780, 45.50804040601273925, 94.94558880294498238 ) ) ;
#12443 = DIRECTION ( 'NONE',  ( -0.3165065846431825980, -0.9485903129789527988, 0.000000000000000000 ) ) ;
#12444 = CARTESIAN_POINT ( 'NONE',  ( -3.850375455727051310, 51.85350431403718119, 79.38294305353919356 ) ) ;
#12445 = CARTESIAN_POINT ( 'NONE',  ( 5.568489401881125289, 48.03437091500646261, 90.57058880123798872 ) ) ;
#12446 = CARTESIAN_POINT ( 'NONE',  ( -8.311663145292943256, 42.89697774700320565, 78.43041451606663372 ) ) ;
#12447 = CARTESIAN_POINT ( 'NONE',  ( 8.628576132315311398, 42.92643779739703547, 77.76019013650333989 ) ) ;
#12448 = EDGE_CURVE ( 'NONE', #12841, #374, #8282, .T. ) ;
#12449 = ORIENTED_EDGE ( 'NONE', *, *, #20534, .T. ) ;
#12450 = CARTESIAN_POINT ( 'NONE',  ( 29.63948732994508006, 36.35905713404685002, 76.90433879953101837 ) ) ;
#12451 = CARTESIAN_POINT ( 'NONE',  ( -4.637383097126852149, 37.03290878947740339, 79.54612747205591461 ) ) ;
#12452 = CARTESIAN_POINT ( 'NONE',  ( 8.909863635552733641, 41.49715104914803021, 76.00786757613292366 ) ) ;
#12453 = CARTESIAN_POINT ( 'NONE',  ( 0.3295378388929664504, 52.35996878549973133, 78.69601710400918648 ) ) ;
#12454 = DIRECTION ( 'NONE',  ( -1.540237394707284467E-16, -1.793354297423764243E-16, 1.000000000000000000 ) ) ;
#12455 = CARTESIAN_POINT ( 'NONE',  ( -4.038468682635965479, 50.97692532282305677, 78.66485665160126928 ) ) ;
#12456 = CARTESIAN_POINT ( 'NONE',  ( -5.945795452124602143, 37.96218137147967298, 53.35433879953099989 ) ) ;
#12457 = DIRECTION ( 'NONE',  ( 1.016439536705157818E-16, 1.000000000000000000, 0.000000000000000000 ) ) ;
#12458 = EDGE_CURVE ( 'NONE', #5674, #4858, #1690, .T. ) ;
#12459 = VERTEX_POINT ( 'NONE', #85 ) ;
#12460 = CARTESIAN_POINT ( 'NONE',  ( -5.508129029085064410, 38.61210022972240097, 78.53742703482498655 ) ) ;
#12461 = CARTESIAN_POINT ( 'NONE',  ( 0.6309698074632331677, 52.36148849043851072, 78.93320637710581877 ) ) ;
#12462 = CARTESIAN_POINT ( 'NONE',  ( 5.895605937740185709, 51.13344329408603528, 78.75475733230618403 ) ) ;
#12463 = CARTESIAN_POINT ( 'NONE',  ( 0.9542774672681346715, 52.35128066847121886, 75.37609433907658740 ) ) ;
#12464 = EDGE_CURVE ( 'NONE', #11154, #3488, #185, .T. ) ;
#12465 = B_SPLINE_CURVE_WITH_KNOTS ( 'NONE', 3,
 ( #2410, #8911, #15075, #707, #15400, #5591, #3579, #13572, #3991, #12097 ),
 .UNSPECIFIED., .F., .F.,
 ( 4, 2, 2, 2, 4 ),
 ( 0.000000000000000000, 0.0001454258534705730479, 0.0002181387802058595718, 0.0002908517069411460957, 0.0005817034138821733629 ),
 .UNSPECIFIED. ) ;
#12466 = ORIENTED_EDGE ( 'NONE', *, *, #18293, .T. ) ;
#12467 = LINE ( 'NONE', #6066, #15658 ) ;
#12468 = CARTESIAN_POINT ( 'NONE',  ( -3.943187491250720544, 40.73580453397070755, 93.14871380294496817 ) ) ;
#12469 = ORIENTED_EDGE ( 'NONE', *, *, #1186, .T. ) ;
#12470 = CARTESIAN_POINT ( 'NONE',  ( 6.691294758883309157, 37.75465145915448062, 78.79551527011911105 ) ) ;
#12471 = CARTESIAN_POINT ( 'NONE',  ( 0.5221537403065015237, 44.16218137147968292, 75.45433879953088763 ) ) ;
#12472 = STYLED_ITEM ( 'NONE', ( #19262 ), #10973 ) ;
#12473 = CARTESIAN_POINT ( 'NONE',  ( 8.263696488377984650, 41.51540230796872066, 78.01079203130994699 ) ) ;
#12474 = DIRECTION ( 'NONE',  ( 1.540237394707284220E-16, 1.793354297423764243E-16, -1.000000000000000000 ) ) ;
#12475 = CARTESIAN_POINT ( 'NONE',  ( 3.357643116058059984, 50.56218137147968861, 96.05433879953096721 ) ) ;
#12476 = CARTESIAN_POINT ( 'NONE',  ( -3.736319852780225048, 36.36732966792004618, 79.18890841331918296 ) ) ;
#12477 = EDGE_LOOP ( 'NONE', ( #10363, #17357, #5646, #11458 ) ) ;
#12478 = LINE ( 'NONE', #2993, #17667 ) ;
#12479 = ORIENTED_EDGE ( 'NONE', *, *, #901, .F. ) ;
#12480 = CARTESIAN_POINT ( 'NONE',  ( 6.208852450660900857, 50.07003620731933324, 77.72233382526972889 ) ) ;
#12481 = CARTESIAN_POINT ( 'NONE',  ( 4.567922609689349045, 52.11414948617044729, 77.12434737327507150 ) ) ;
#12482 = CARTESIAN_POINT ( 'NONE',  ( 0.5221537403064999694, 39.16218137147969003, 92.45433879953097289 ) ) ;
#12483 = FACE_OUTER_BOUND ( 'NONE', #15122, .T. ) ;
#12484 = CARTESIAN_POINT ( 'NONE',  ( 28.52215374030649642, 40.36218137147969287, 87.65433879953101837 ) ) ;
#12485 = DIRECTION ( 'NONE',  ( -0.000000000000000000, -0.000000000000000000, 1.000000000000000000 ) ) ;
#12486 = VECTOR ( 'NONE', #13430, 1000.000000000000000 ) ;
#12487 = VERTEX_POINT ( 'NONE', #10092 ) ;
#12488 = ORIENTED_EDGE ( 'NONE', *, *, #8700, .F. ) ;
#12489 = CARTESIAN_POINT ( 'NONE',  ( -3.566438244846301231, 38.23101125920473464, 76.81463291717793140 ) ) ;
#12490 = CARTESIAN_POINT ( 'NONE',  ( -0.8237052942265477018, 49.18499566818285018, 91.19558879953099506 ) ) ;
#12491 = CARTESIAN_POINT ( 'NONE',  ( 4.634072907867718527, 52.06528692560263494, 75.88092117868445996 ) ) ;
#12492 = ORIENTED_EDGE ( 'NONE', *, *, #11173, .T. ) ;
#12493 = EDGE_CURVE ( 'NONE', #140, #14499, #11789, .T. ) ;
#12494 = CARTESIAN_POINT ( 'NONE',  ( -4.740836738068939127, 51.21721328354402658, 79.54427050475041483 ) ) ;
#12495 = CARTESIAN_POINT ( 'NONE',  ( 0.5221537403065364957, 44.16218137147969003, 123.5543387995310098 ) ) ;
#12496 = VERTEX_POINT ( 'NONE', #3278 ) ;
#12497 = VECTOR ( 'NONE', #15657, 1000.000000000000000 ) ;
#12498 = CARTESIAN_POINT ( 'NONE',  ( 4.393996117251955269, 36.11308595931626542, 76.73963291717792856 ) ) ;
#12499 = CARTESIAN_POINT ( 'NONE',  ( 1.445335398664440607, 38.34581663015914188, 95.05433879953095300 ) ) ;
#12500 = EDGE_CURVE ( 'NONE', #14257, #5774, #11693, .T. ) ;
#12501 = ORIENTED_EDGE ( 'NONE', *, *, #8197, .T. ) ;
#12502 = CARTESIAN_POINT ( 'NONE',  ( -3.943187491250720544, 40.73580453397070755, 92.83621379953099506 ) ) ;
#12503 = CARTESIAN_POINT ( 'NONE',  ( 0.6699824260347926330, 52.35356008955702123, 78.92081865479288183 ) ) ;
#12504 = VECTOR ( 'NONE', #4320, 1000.000000000000227 ) ;
#12505 = EDGE_LOOP ( 'NONE', ( #15988, #19932, #7686, #5976 ) ) ;
#12506 = CARTESIAN_POINT ( 'NONE',  ( -2.712716146932703687, 39.96922920035118665, 92.45433879953094447 ) ) ;
#12507 = FACE_OUTER_BOUND ( 'NONE', #2508, .T. ) ;
#12508 = ADVANCED_FACE ( 'NONE', ( #8171 ), #9995, .F. ) ;
#12509 = CARTESIAN_POINT ( 'NONE',  ( -4.622577041588897373, 46.56120873422322859, 95.06371379782397923 ) ) ;
#12510 = EDGE_CURVE ( 'NONE', #14796, #8473, #18168, .T. ) ;
#12511 = CARTESIAN_POINT ( 'NONE',  ( 5.074465183246153366, 37.34623967253333632, 76.70433879953087342 ) ) ;
#12512 = CARTESIAN_POINT ( 'NONE',  ( 5.677877744449962627, 51.29427033984291029, 78.92241520643889885 ) ) ;
#12513 = AXIS2_PLACEMENT_3D ( 'NONE', #3393, #8297, #11290 ) ;
#12514 = CARTESIAN_POINT ( 'NONE',  ( -3.513222121926658392, 37.12736930804990010, 77.68963291717793140 ) ) ;
#12515 = VERTEX_POINT ( 'NONE', #16262 ) ;
#12516 = CARTESIAN_POINT ( 'NONE',  ( 1.374762211169257897, 52.92186301335429732, 76.79053302980838680 ) ) ;
#12517 = EDGE_LOOP ( 'NONE', ( #11412, #4506, #4002, #17701, #12043 ) ) ;
#12518 = CARTESIAN_POINT ( 'NONE',  ( 6.780993214391527246, 50.47944337839869888, 75.76076839092205262 ) ) ;
#12519 = CARTESIAN_POINT ( 'NONE',  ( -0.9307445186194918119, 52.23244111531224831, 76.43472685704757907 ) ) ;
#12520 = CARTESIAN_POINT ( 'NONE',  ( 6.198496396448986090, 45.68315280215533392, 95.33621380123798872 ) ) ;
#12521 = ORIENTED_EDGE ( 'NONE', *, *, #17925, .T. ) ;
#12522 = ORIENTED_EDGE ( 'NONE', *, *, #17142, .T. ) ;
#12523 = CARTESIAN_POINT ( 'NONE',  ( -4.238909561394200942, 37.66340538711140340, 75.36060488990274564 ) ) ;
#12524 = CARTESIAN_POINT ( 'NONE',  ( 5.370821505553895925, 50.60706540930752340, 79.54761434581399726 ) ) ;
#12525 = ORIENTED_EDGE ( 'NONE', *, *, #11446, .T. ) ;
#12526 = CARTESIAN_POINT ( 'NONE',  ( 5.270041363239100995, 50.68150764076370507, 79.54768974400036541 ) ) ;
#12527 = CARTESIAN_POINT ( 'NONE',  ( 8.818545868716455516, 41.22346590884859552, 77.48357784852399277 ) ) ;
#12528 = CARTESIAN_POINT ( 'NONE',  ( 0.7582201636353298468, 49.56899138526064519, 90.53246379953097289 ) ) ;
#12529 = VECTOR ( 'NONE', #3849, 1000.000000000000114 ) ;
#12530 = ORIENTED_EDGE ( 'NONE', *, *, #5873, .F. ) ;
#12531 = CARTESIAN_POINT ( 'NONE',  ( 6.120570592859386316, 50.15433377453709340, 75.51955991867161799 ) ) ;
#12532 = CARTESIAN_POINT ( 'NONE',  ( -7.677846259693483333, 47.36218137147966445, 80.55433879953099563 ) ) ;
#12533 = PLANE ( 'NONE',  #328 ) ;
#12534 = EDGE_CURVE ( 'NONE', #8576, #15405, #12004, .T. ) ;
#12535 = CARTESIAN_POINT ( 'NONE',  ( 5.568489401881125289, 48.03437091500646261, 95.41433880123797451 ) ) ;
#12536 = LINE ( 'NONE', #19022, #3992 ) ;
#12537 =( BOUNDED_CURVE ( )  B_SPLINE_CURVE ( 2, ( #742, #2024, #8521, #2340, #19983, #15006, #7227, #2451, #5202, #15433, #428 ),
 .UNSPECIFIED., .F., .F. ) 
 B_SPLINE_CURVE_WITH_KNOTS ( ( 3, 2, 2, 2, 2, 3 ),
 ( 0.3472607999482700269, 0.3645715623395309746, 0.3906123882209271425, 0.4166532141023233660, 0.4426940399837194784, 0.4514241053481902743 ),
 .UNSPECIFIED. ) 
 CURVE ( )  GEOMETRIC_REPRESENTATION_ITEM ( )  RATIONAL_B_SPLINE_CURVE ( ( 0.9660722130358361248, 0.9493985585629908242, 1.000000000000000000, 0.9238795325112867385, 1.000000000000000000, 0.9238795325112867385, 1.000000000000000000, 0.9238795325112867385, 1.000000000000000000, 0.9744809684693873653, 0.9660722094251321668 ) ) 
 REPRESENTATION_ITEM ( '' )  );
#12538 = CARTESIAN_POINT ( 'NONE',  ( 2.722153740306501479, 44.16218137147969003, 50.15433879953098995 ) ) ;
#12539 = DIRECTION ( 'NONE',  ( 1.000000000000000000, 0.000000000000000000, 0.000000000000000000 ) ) ;
#12540 = CARTESIAN_POINT ( 'NONE',  ( -7.382281811460246423, 40.29405236905069643, 79.07682695550360563 ) ) ;
#12541 = CARTESIAN_POINT ( 'NONE',  ( 8.951736416449948663, 41.62264642985666541, 78.48252796260671005 ) ) ;
#12542 = VECTOR ( 'NONE', #2054, 1000.000000000000000 ) ;
#12543 = CARTESIAN_POINT ( 'NONE',  ( -0.9304578138521076847, 52.97982027947340100, 78.32762347114741885 ) ) ;
#12544 = CARTESIAN_POINT ( 'NONE',  ( 5.722153675948534080, 44.84677459912131070, 94.92075777718328311 ) ) ;
#12545 = DIRECTION ( 'NONE',  ( 0.9485903129789527988, -0.3165065846431829311, 8.934458285744989980E-17 ) ) ;
#12546 = LINE ( 'NONE', #17336, #4834 ) ;
#12547 =( NAMED_UNIT ( * ) PLANE_ANGLE_UNIT ( ) SI_UNIT ( $, .RADIAN. ) );
#12548 = ORIENTED_EDGE ( 'NONE', *, *, #11974, .F. ) ;
#12549 = CARTESIAN_POINT ( 'NONE',  ( -7.294099066665586051, 42.13140977396874831, 79.52797380487967871 ) ) ;
#12550 = CARTESIAN_POINT ( 'NONE',  ( 5.341647780419348734, 37.53715857429408231, 75.97340568087561508 ) ) ;
#12551 = ORIENTED_EDGE ( 'NONE', *, *, #3647, .T. ) ;
#12552 = CYLINDRICAL_SURFACE ( 'NONE', #10776, 6.999999999999999112 ) ;
#12553 = DIRECTION ( 'NONE',  ( -1.000000000000000000, 1.110223024625156540E-16, -1.779391786395883043E-16 ) ) ;
#12554 = DIRECTION ( 'NONE',  ( -1.000000000000000000, 1.110223024625156540E-16, -1.779391786395883043E-16 ) ) ;
#12555 = CARTESIAN_POINT ( 'NONE',  ( 8.947628219434415442, 41.61033390278195299, 77.32525259820312158 ) ) ;
#12556 = AXIS2_PLACEMENT_3D ( 'NONE', #20962, #15798, #19384 ) ;
#12557 = CARTESIAN_POINT ( 'NONE',  ( -4.056262464355276265, 50.96498501010217552, 78.79673532154967575 ) ) ;
#12558 = CARTESIAN_POINT ( 'NONE',  ( 5.398882651910504649, 50.75441279359508684, 77.28963291717792572 ) ) ;
#12559 = VECTOR ( 'NONE', #4746, 1000.000000000000114 ) ;
#12560 = CLOSED_SHELL ( 'NONE', ( #7538, #20788, #18971, #17830, #802, #644, #6897, #14470, #14126, #9381, #3123, #7920, #18432, #3062, #6738, #17947, #11600, #3089, #2484, #13524, #10922, #12275, #8835, #10442, #7024, #2444, #2888, #19016, #11213, #3128, #13010, #9770, #9064, #380, #11432, #6353, #15373, #3677, #2053, #14336, #5009, #17304, #9118, #19511, #20777, #9192, #11317, #13788, #9279, #19851, #16009, #20088, #18581, #118, #14670, #18973, #809, #145, #14812, #1391 ) ) ;
#12561 = ORIENTED_EDGE ( 'NONE', *, *, #13418, .T. ) ;
#12562 = CARTESIAN_POINT ( 'NONE',  ( -5.953540064417265576, 38.00510092317821176, 78.67637590524894620 ) ) ;
#12563 = EDGE_CURVE ( 'NONE', #11086, #6021, #19950, .T. ) ;
#12564 = VECTOR ( 'NONE', #14519, 1000.000000000000000 ) ;
#12565 = CARTESIAN_POINT ( 'NONE',  ( 0.5221537403065015237, 44.16218137147968292, 75.45433879953088763 ) ) ;
#12566 = CARTESIAN_POINT ( 'NONE',  ( 5.590052860727733552, 36.96774431777176062, 78.26671861549210973 ) ) ;
#12567 = AXIS2_PLACEMENT_3D ( 'NONE', #1227, #12811, #6310 ) ;
#12568 = VECTOR ( 'NONE', #6197, 1000.000000000000227 ) ;
#12569 = EDGE_LOOP ( 'NONE', ( #1376, #14906, #2097, #12324 ) ) ;
#12570 = CARTESIAN_POINT ( 'NONE',  ( -3.777846259693486974, 51.36218137147968577, 93.55433879953098142 ) ) ;
#12571 = CARTESIAN_POINT ( 'NONE',  ( 6.102441102155617969, 43.42752260303680600, 93.61746380294498238 ) ) ;
#12572 = ORIENTED_EDGE ( 'NONE', *, *, #19242, .T. ) ;
#12573 = CARTESIAN_POINT ( 'NONE',  ( -5.405939962049822967, 49.82766502745145232, 78.10580938776615767 ) ) ;
#12574 = EDGE_CURVE ( 'NONE', #5140, #5376, #5072, .T. ) ;
#12575 = CARTESIAN_POINT ( 'NONE',  ( -4.677846259693498432, 44.16218137147969003, 93.95661078214054385 ) ) ;
#12576 = CONICAL_SURFACE ( 'NONE', #12905, 4.000000000000003553, 0.7853981633974460586 ) ;
#12577 = CARTESIAN_POINT ( 'NONE',  ( 5.760694563098077481, 51.23309689197249384, 79.54845644658969661 ) ) ;
#12578 = FACE_OUTER_BOUND ( 'NONE', #18571, .T. ) ;
#12579 = CARTESIAN_POINT ( 'NONE',  ( 0.6297410054736833906, 52.96530755180469896, 75.97323462179006981 ) ) ;
#12580 = CARTESIAN_POINT ( 'NONE',  ( -3.547760446584435012, 36.22804843019940790, 78.70659543854199569 ) ) ;
#12581 = VERTEX_POINT ( 'NONE', #16371 ) ;
#12582 = DIRECTION ( 'NONE',  ( -0.3165065846431825980, -0.9485903129789530208, 0.000000000000000000 ) ) ;
#12583 = CARTESIAN_POINT ( 'NONE',  ( -3.628867371436363509, 48.69222599884265179, 92.32933879782399345 ) ) ;
#12584 = VERTEX_POINT ( 'NONE', #1996 ) ;
#12585 = CARTESIAN_POINT ( 'NONE',  ( -5.154188915835984375, 42.64120994080404614, 93.46121380123797451 ) ) ;
#12586 = AXIS2_PLACEMENT_3D ( 'NONE', #7645, #15420, #835 ) ;
#12587 = VECTOR ( 'NONE', #13959, 1000.000000000000000 ) ;
#12588 = CARTESIAN_POINT ( 'NONE',  ( -2.416137431568557314, 39.07291177436112406, 94.86746380123797451 ) ) ;
#12589 = CARTESIAN_POINT ( 'NONE',  ( 5.427780505986065762, 36.85179043424346190, 77.43080938776617472 ) ) ;
#12590 = CARTESIAN_POINT ( 'NONE',  ( 5.052198367669452850, 48.31320248322254685, 94.67308879782399345 ) ) ;
#12591 = CARTESIAN_POINT ( 'NONE',  ( -7.286377378278460881, 41.68676597530894412, 78.93669174070734584 ) ) ;
#12592 = B_SPLINE_SURFACE_WITH_KNOTS ( 'NONE', 3, 1, ( 
 ( #999, #687 ),
 ( #12295, #20240 ),
 ( #2600, #2502 ),
 ( #9096, #12182 ),
 ( #8777, #8993 ),
 ( #7166, #15266 ),
 ( #20140, #5573 ),
 ( #12076, #3970 ),
 ( #17382, #19279 ),
 ( #20865, #6399 ),
 ( #9409, #17486 ),
 ( #7906, #14395 ),
 ( #12796, #17582 ),
 ( #19086, #7702 ),
 ( #15898, #12598 ),
 ( #4495, #1212 ),
 ( #11218, #11115 ),
 ( #11015, #6091 ),
 ( #19177, #1318 ),
 ( #18976, #15800 ),
 ( #4387, #17797 ),
 ( #4692, #7801 ),
 ( #17692, #2912 ),
 ( #3011, #2809 ),
 ( #3221, #10912 ),
 ( #14288, #20764 ),
 ( #12700, #16205 ) ),
 .UNSPECIFIED., .F., .F., .F.,
 ( 4, 1, 1, 1, 1, 1, 1, 1, 1, 1, 1, 1, 1, 1, 1, 1, 1, 1, 1, 1, 1, 1, 1, 1, 4 ),
 ( 2, 2 ),
 ( 0.000000000000000000, 0.04692756115915790172, 0.09175764483083305445, 0.1348320239538815524, 0.1755606184341063081, 0.2149124488236470176, 0.2520401868719510108, 0.2875439711136699161, 0.3211732624427411364, 0.3845494416143411254, 0.4434775415870848558, 0.4991878644837567380, 0.5522905917841786083, 0.6030460594100006677, 0.6509449284921694501, 0.6968976034913704209, 0.7406443924834601455, 0.7634319837341128068, 0.7890572409307390345, 0.8171397283500007047, 0.8480511511928767732, 0.8815178987434894031, 0.9182285974223420855, 0.9576130192529551666, 1.000000000000000000 ),
 ( 0.000000000000000000, 1.000000000000000000 ),
 .UNSPECIFIED. ) ;
#12593 = CIRCLE ( 'NONE', #3409, 8.800000000000000711 ) ;
#12594 = ADVANCED_FACE ( 'NONE', ( #18265 ), #11590, .F. ) ;
#12595 = ORIENTED_EDGE ( 'NONE', *, *, #15896, .F. ) ;
#12596 = CARTESIAN_POINT ( 'NONE',  ( 0.5221537403065064087, 50.16218137147969713, 77.15433879953100416 ) ) ;
#12597 = ORIENTED_EDGE ( 'NONE', *, *, #7622, .T. ) ;
#12598 = CARTESIAN_POINT ( 'NONE',  ( -3.119948039661358585, 51.45566542062479698, 75.79042024895623797 ) ) ;
#12599 = CARTESIAN_POINT ( 'NONE',  ( 4.394343283833276992, 39.11584570990505938, 92.75808880123797451 ) ) ;
#12600 = CARTESIAN_POINT ( 'NONE',  ( 8.617049974001410817, 45.47086815721986142, 79.23054824294796106 ) ) ;
#12601 = CARTESIAN_POINT ( 'NONE',  ( 8.787829143201870252, 41.13140593384865440, 77.80727997600146750 ) ) ;
#12602 = ORIENTED_EDGE ( 'NONE', *, *, #14809, .T. ) ;
#12603 = CARTESIAN_POINT ( 'NONE',  ( -5.484081776600456593, 50.68611759094706315, 79.26884812577799266 ) ) ;
#12604 = LINE ( 'NONE', #7607, #17429 ) ;
#12605 = CARTESIAN_POINT ( 'NONE',  ( 4.425132644269478277, 36.13533498154198043, 76.25036098622081226 ) ) ;
#12606 = EDGE_CURVE ( 'NONE', #16873, #2184, #5530, .T. ) ;
#12607 = CARTESIAN_POINT ( 'NONE',  ( 5.228185313790076449, 50.87180408165244927, 76.07177712439327877 ) ) ;
#12608 = EDGE_LOOP ( 'NONE', ( #14628, #11696, #5821, #8798 ) ) ;
#12609 = CARTESIAN_POINT ( 'NONE',  ( 3.948530577815479337, 39.69684013992245752, 93.14871379953099506 ) ) ;
#12610 = CARTESIAN_POINT ( 'NONE',  ( 0.8172236777486411308, 52.96375677797878012, 78.79200666326234170 ) ) ;
#12611 = EDGE_CURVE ( 'NONE', #2112, #13012, #3777, .T. ) ;
#12612 = ORIENTED_EDGE ( 'NONE', *, *, #11849, .F. ) ;
#12613 = CARTESIAN_POINT ( 'NONE',  ( -2.530020917761411692, 39.85184329928002001, 92.45433879953093026 ) ) ;
#12614 = DIRECTION ( 'NONE',  ( 0.3165065846431826535, 0.9485903129789529098, 2.188653791613874008E-16 ) ) ;
#12615 = CARTESIAN_POINT ( 'NONE',  ( -1.419351766502867429, 49.49642391118513274, 92.40746379782397923 ) ) ;
#12616 = CARTESIAN_POINT ( 'NONE',  ( 5.144371138689071365, 37.39619190887245992, 76.03636210503219672 ) ) ;
#12618 = ADVANCED_FACE ( 'NONE', ( #6974 ), #5642, .F. ) ;
#12617 = CARTESIAN_POINT ( 'NONE',  ( 5.599463258324014703, 51.35219196201597214, 78.62371398036725623 ) ) ;
#12619 = ADVANCED_FACE ( 'NONE', ( #12321 ), #8803, .F. ) ;
#12620 = CARTESIAN_POINT ( 'NONE',  ( -3.752498811055299477, 36.37928041266965806, 77.59103917682324436 ) ) ;
#12621 = EDGE_CURVE ( 'NONE', #18224, #3380, #15406, .T. ) ;
#12622 = ORIENTED_EDGE ( 'NONE', *, *, #13819, .F. ) ;
#12623 = CARTESIAN_POINT ( 'NONE',  ( 1.830036527069967445, 52.86461688513685431, 76.99776405956157532 ) ) ;
#12624 = ORIENTED_EDGE ( 'NONE', *, *, #1024, .F. ) ;
#12625 = DIRECTION ( 'NONE',  ( 6.308085367188358884E-15, 3.469446951953626515E-16, 1.000000000000000000 ) ) ;
#12626 = EDGE_CURVE ( 'NONE', #16572, #7590, #599, .T. ) ;
#12627 = CARTESIAN_POINT ( 'NONE',  ( 5.631785411401764918, 36.99756487055721976, 77.76022115247205591 ) ) ;
#12628 = CARTESIAN_POINT ( 'NONE',  ( 4.454354847297358866, 39.79502961122975790, 90.27410626197791998 ) ) ;
#12629 = CARTESIAN_POINT ( 'NONE',  ( 31.07218010054375412, 42.96218137147968008, 69.80574467885101342 ) ) ;
#12630 = ORIENTED_EDGE ( 'NONE', *, *, #20256, .F. ) ;
#12631 = ORIENTED_EDGE ( 'NONE', *, *, #18724, .T. ) ;
#12632 = CIRCLE ( 'NONE', #15743, 3.999999999999996447 ) ;
#12633 = DIRECTION ( 'NONE',  ( 3.620524460287510065E-17, -1.000000000000000000, -7.183611964723545059E-17 ) ) ;
#12634 = CARTESIAN_POINT ( 'NONE',  ( -4.546230963980876005, 36.96557838055436207, 76.09208750614521932 ) ) ;
#12635 = DIRECTION ( 'NONE',  ( -0.5941461771851783702, -0.8043570849667693867, -2.357623395011398763E-16 ) ) ;
#12636 = VECTOR ( 'NONE', #13718, 1000.000000000000000 ) ;
#12637 = ORIENTED_EDGE ( 'NONE', *, *, #7938, .T. ) ;
#12638 = ADVANCED_FACE ( 'NONE', ( #3896 ), #7080, .T. ) ;
#12639 = CARTESIAN_POINT ( 'NONE',  ( 4.154601481547989472, 51.50543814870972881, 78.70655549710109256 ) ) ;
#12640 = CARTESIAN_POINT ( 'NONE',  ( 8.286663948227678489, 41.54943773017198794, 77.52392363563762956 ) ) ;
#12641 = CARTESIAN_POINT ( 'NONE',  ( -4.176309363623029292, 42.45208065485131499, 92.17308879953097289 ) ) ;
#12642 = ORIENTED_EDGE ( 'NONE', *, *, #4412, .F. ) ;
#12643 = CARTESIAN_POINT ( 'NONE',  ( -1.306251101200022857, 49.87752504164858891, 61.32593395802449265 ) ) ;
#12644 = CARTESIAN_POINT ( 'NONE',  ( -7.176555495732481305, 41.78858715306228078, 79.54845644658969661 ) ) ;
#12645 = CARTESIAN_POINT ( 'NONE',  ( 6.243933501899546101, 38.28785586627228099, 75.68656110871486931 ) ) ;
#12646 = CARTESIAN_POINT ( 'NONE',  ( 3.460444912181559474, 49.25145096859824889, 91.89871380123798872 ) ) ;
#12647 = DIRECTION ( 'NONE',  ( 0.000000000000000000, 0.000000000000000000, 1.000000000000000000 ) ) ;
#12648 = FACE_OUTER_BOUND ( 'NONE', #7552, .T. ) ;
#12649 = VECTOR ( 'NONE', #7111, 1000.000000000000000 ) ;
#12650 = CARTESIAN_POINT ( 'NONE',  ( -1.477846259693506914, 47.62628298661743997, 85.15433879953098995 ) ) ;
#12651 = EDGE_CURVE ( 'NONE', #12841, #17122, #8216, .T. ) ;
#12652 = DIRECTION ( 'NONE',  ( -1.540237394707284467E-16, -1.793354297423764243E-16, 1.000000000000000000 ) ) ;
#12653 = AXIS2_PLACEMENT_3D ( 'NONE', #8937, #13500, #5402 ) ;
#12654 = CARTESIAN_POINT ( 'NONE',  ( 27.03948732994508930, 45.16218137147969003, 76.90433879953101837 ) ) ;
#12655 = CARTESIAN_POINT ( 'NONE',  ( -4.180832706968435453, 37.44488997341807845, 76.12122195298280758 ) ) ;
#12656 = CARTESIAN_POINT ( 'NONE',  ( 11.22215374030650281, 42.76218137147968434, 78.80433879953099563 ) ) ;
#12657 = EDGE_CURVE ( 'NONE', #18041, #16139, #5497, .T. ) ;
#12658 = CARTESIAN_POINT ( 'NONE',  ( 5.563409226749892689, 51.37882362279480475, 76.27120023672567584 ) ) ;
#12659 = CARTESIAN_POINT ( 'NONE',  ( 8.661599634585138929, 45.15687757339797059, 72.45433879953087342 ) ) ;
#12660 = ORIENTED_EDGE ( 'NONE', *, *, #17707, .F. ) ;
#12661 = EDGE_LOOP ( 'NONE', ( #4691, #14237, #12492, #8287 ) ) ;
#12662 = VECTOR ( 'NONE', #20164, 1000.000000000000000 ) ;
#12663 = CARTESIAN_POINT ( 'NONE',  ( -1.477846259693499364, 47.62628298661744708, 69.15433879953098995 ) ) ;
#12664 = DIRECTION ( 'NONE',  ( -0.009567942452870459302, 0.9999542261909885044, 1.778535306010345054E-16 ) ) ;
#12665 = CARTESIAN_POINT ( 'NONE',  ( 5.077125919649112085, 37.34365979239193933, 77.51217538217308345 ) ) ;
#12666 = VECTOR ( 'NONE', #18436, 1000.000000000000000 ) ;
#12667 = CARTESIAN_POINT ( 'NONE',  ( 0.3744753729714065948, 52.36086421975554828, 78.83587839956341270 ) ) ;
#12668 = CARTESIAN_POINT ( 'NONE',  ( 5.315345751398379726, 50.80894264282942885, 77.96371040190514634 ) ) ;
#12669 = CARTESIAN_POINT ( 'NONE',  ( -6.709328582052544121, 40.29621921162754461, 72.45433879953085921 ) ) ;
#12670 = CARTESIAN_POINT ( 'NONE',  ( 35.92215374030650565, 51.36218137147967866, 93.55433879953098142 ) ) ;
#12671 = DIRECTION ( 'NONE',  ( 1.084202172485505420E-16, 1.000000000000000000, 0.000000000000000000 ) ) ;
#12672 = ORIENTED_EDGE ( 'NONE', *, *, #18192, .T. ) ;
#12673 = CARTESIAN_POINT ( 'NONE',  ( 8.787829143201872029, 41.13140593384864729, 78.45948585835439815 ) ) ;
#12674 = AXIS2_PLACEMENT_3D ( 'NONE', #13149, #8466, #14949 ) ;
#12675 = CARTESIAN_POINT ( 'NONE',  ( -5.435385416347992660, 50.72091422709593189, 79.30596685730465367 ) ) ;
#12676 = CARTESIAN_POINT ( 'NONE',  ( 5.275347668770276499, 50.84403652138585272, 78.87333753819284254 ) ) ;
#12677 = ORIENTED_EDGE ( 'NONE', *, *, #11540, .T. ) ;
#12678 = DIRECTION ( 'NONE',  ( -3.893792155548169402E-16, -7.183611964723547524E-17, 1.000000000000000000 ) ) ;
#12679 = CARTESIAN_POINT ( 'NONE',  ( -2.077846259693550746, 39.65884927180063357, 91.97683880294496817 ) ) ;
#12680 = ORIENTED_EDGE ( 'NONE', *, *, #2166, .T. ) ;
#12681 = CARTESIAN_POINT ( 'NONE',  ( 5.541571994271107471, 50.64183843016825648, 78.67852979887695142 ) ) ;
#12682 = CARTESIAN_POINT ( 'NONE',  ( -0.9184319840176534688, 52.97850019102069297, 76.32609705745309725 ) ) ;
#12683 = CARTESIAN_POINT ( 'NONE',  ( -4.477846259693498254, 36.96218137147968008, 53.35433879953099989 ) ) ;
#12684 = CARTESIAN_POINT ( 'NONE',  ( 2.522153740306508407, 50.16218137147969713, 67.55433879953099563 ) ) ;
#12685 = CARTESIAN_POINT ( 'NONE',  ( 0.7882770238055200052, 52.35261454525205238, 76.04568394904065087 ) ) ;
#12686 = CARTESIAN_POINT ( 'NONE',  ( -1.376885767552595619, 38.47063949360596524, 82.45433879953087342 ) ) ;
#12687 = ORIENTED_EDGE ( 'NONE', *, *, #2039, .T. ) ;
#12688 = CARTESIAN_POINT ( 'NONE',  ( 8.873269659708348911, 41.38747658206386149, 75.97261045075327957 ) ) ;
#12689 = VECTOR ( 'NONE', #8971, 1000.000000000000227 ) ;
#12690 = ORIENTED_EDGE ( 'NONE', *, *, #16049, .T. ) ;
#12691 = CARTESIAN_POINT ( 'NONE',  ( -0.9988176903691428077, 49.83852402762217082, 93.14871380123798872 ) ) ;
#12692 = DIRECTION ( 'NONE',  ( 1.540237394707284220E-16, 1.793354297423764243E-16, -1.000000000000000000 ) ) ;
#12693 = CARTESIAN_POINT ( 'NONE',  ( 0.3501649423846716624, 52.36039128232832240, 76.08536861688374131 ) ) ;
#12694 = CARTESIAN_POINT ( 'NONE',  ( 5.835344820533724608, 37.14302097153727544, 76.09175310361966638 ) ) ;
#12695 = LINE ( 'NONE', #6393, #1778 ) ;
#12696 = VERTEX_POINT ( 'NONE', #10520 ) ;
#12697 = CARTESIAN_POINT ( 'NONE',  ( 4.791956560326987358, 51.94866463147243962, 77.83360891957636341 ) ) ;
#12698 = VERTEX_POINT ( 'NONE', #10313 ) ;
#12699 = VECTOR ( 'NONE', #12692, 1000.000000000000000 ) ;
#12700 = CARTESIAN_POINT ( 'NONE',  ( -3.349688636638950889, 52.21127678364309332, 76.69845644658968808 ) ) ;
#12701 = CARTESIAN_POINT ( 'NONE',  ( -2.416137431568557314, 39.07291177436112406, 93.77371380123797451 ) ) ;
#12702 = CARTESIAN_POINT ( 'NONE',  ( 4.561823949912076515, 52.11865432047892455, 76.17419329630023128 ) ) ;
#12703 = ORIENTED_EDGE ( 'NONE', *, *, #3550, .F. ) ;
#12704 = CARTESIAN_POINT ( 'NONE',  ( -5.233355322855509861, 49.94533053554986424, 79.06611278947218580 ) ) ;
#12705 = CARTESIAN_POINT ( 'NONE',  ( 8.889576793745449734, 46.88836537034026719, 78.73595644658969661 ) ) ;
#12706 = CARTESIAN_POINT ( 'NONE',  ( -4.156427319950603660, 37.43228207296065335, 78.58080938776616620 ) ) ;
#12707 = CARTESIAN_POINT ( 'NONE',  ( -4.405821937837398394, 51.45660259411479132, 78.79092181577959764 ) ) ;
#12708 = EDGE_CURVE ( 'NONE', #12698, #3704, #17103, .T. ) ;
#12709 = CARTESIAN_POINT ( 'NONE',  ( -0.4699484075729999932, 51.36218137147968577, 83.03825919817350609 ) ) ;
#12710 = EDGE_LOOP ( 'NONE', ( #1802, #18478, #11699, #16034 ) ) ;
#12711 = CARTESIAN_POINT ( 'NONE',  ( -4.225735884248155827, 46.53332982581555655, 92.55433879953098142 ) ) ;
#12712 = CARTESIAN_POINT ( 'NONE',  ( 3.460444912181559474, 49.25145096859824889, 91.89871380123798872 ) ) ;
#12713 = ORIENTED_EDGE ( 'NONE', *, *, #4930, .F. ) ;
#12714 = CARTESIAN_POINT ( 'NONE',  ( 4.203679381925226721, 51.46918628067947310, 78.02172882224894579 ) ) ;
#12715 = CYLINDRICAL_SURFACE ( 'NONE', #10902, 0.5999999999999894307 ) ;
#12716 = LINE ( 'NONE', #11237, #20027 ) ;
#12717 = CARTESIAN_POINT ( 'NONE',  ( 0.2541436421823696223, 38.02374091943176637, 95.45433879782399345 ) ) ;
#12718 = CARTESIAN_POINT ( 'NONE',  ( 5.081160855019016154, 37.35102415443803636, 76.36627918048426977 ) ) ;
#12719 = DIRECTION ( 'NONE',  ( -1.779391786395883536E-16, -5.922860397471806844E-17, 1.000000000000000000 ) ) ;
#12720 = CARTESIAN_POINT ( 'NONE',  ( -3.067799679179274541, 36.79835369230286091, 77.03801799112748938 ) ) ;
#12721 = ADVANCED_FACE ( 'NONE', ( #2419 ), #2625, .F. ) ;
#12722 = ORIENTED_EDGE ( 'NONE', *, *, #7, .F. ) ;
#12723 = CARTESIAN_POINT ( 'NONE',  ( -7.125180600693382438, 47.12171300294919973, 78.21942560846048309 ) ) ;
#12724 = ORIENTED_EDGE ( 'NONE', *, *, #14818, .F. ) ;
#12725 = B_SPLINE_CURVE_WITH_KNOTS ( 'NONE', 3,
 ( #1845, #8329, #1937, #6716, #19699, #4904, #13223, #16732, #3320, #5011, #19802, #6508, #11840, #2047, #9825, #11425 ),
 .UNSPECIFIED., .F., .F.,
 ( 4, 2, 2, 2, 2, 2, 2, 4 ),
 ( 0.000000000000000000, 0.0003384078081585416482, 0.0005076117122378233414, 0.0006768156163171051972, 0.0007614175683567383189, 0.0008460195203963712237, 0.001015223424475636925, 0.001353631232634169845 ),
 .UNSPECIFIED. ) ;
#12726 = CARTESIAN_POINT ( 'NONE',  ( -7.677846259693485109, 51.36218137147968577, 95.05433879953098142 ) ) ;
#12727 = CARTESIAN_POINT ( 'NONE',  ( -7.077609990433002096, 44.22210830145579763, 75.45433879953087342 ) ) ;
#12728 = CARTESIAN_POINT ( 'NONE',  ( 8.953205446347402230, 41.62704920565285249, 79.54154676390322720 ) ) ;
#12729 = EDGE_CURVE ( 'NONE', #13088, #15854, #12207, .T. ) ;
#12730 = CARTESIAN_POINT ( 'NONE',  ( -8.310158986959008232, 42.88687749725123410, 76.06610350541322418 ) ) ;
#12731 = VERTEX_POINT ( 'NONE', #18689 ) ;
#12732 = DIRECTION ( 'NONE',  ( -0.3165065846431826535, -0.9485903129789527988, 0.000000000000000000 ) ) ;
#12733 = VERTEX_POINT ( 'NONE', #4105 ) ;
#12734 = CARTESIAN_POINT ( 'NONE',  ( -3.607357127890974180, 36.27207009797979254, 75.89423958357750166 ) ) ;
#12735 = DIRECTION ( 'NONE',  ( -0.9539696396349525154, 0.2999031954727373050, -9.315070279690336121E-17 ) ) ;
#12736 = CARTESIAN_POINT ( 'NONE',  ( -5.405939962049822078, 49.82766502745145942, 76.76022115247205591 ) ) ;
#12737 = EDGE_LOOP ( 'NONE', ( #20950, #6350, #10094, #6757 ) ) ;
#12738 = CARTESIAN_POINT ( 'NONE',  ( -4.545392591669653370, 36.96495910869975177, 77.09144163344554102 ) ) ;
#12739 = EDGE_CURVE ( 'NONE', #1868, #13402, #2526, .T. ) ;
#12740 = CARTESIAN_POINT ( 'NONE',  ( 0.5221537403065010796, 44.16218137147968292, 78.25433879953088478 ) ) ;
#12741 = EDGE_CURVE ( 'NONE', #10971, #6648, #2786, .T. ) ;
#12742 = ORIENTED_EDGE ( 'NONE', *, *, #12252, .F. ) ;
#12743 = LINE ( 'NONE', #9766, #1248 ) ;
#12744 = SURFACE_STYLE_FILL_AREA ( #17528 ) ;
#12745 = CARTESIAN_POINT ( 'NONE',  ( 5.706391565287319168, 37.80821467551069048, 75.39252012644811884 ) ) ;
#12746 = CARTESIAN_POINT ( 'NONE',  ( 5.611423337425062385, 41.22389019960463230, 92.83621380123797451 ) ) ;
#12747 = EDGE_CURVE ( 'NONE', #5582, #18174, #1032, .T. ) ;
#12748 = CARTESIAN_POINT ( 'NONE',  ( -5.799282478806809138, 50.46088670938467402, 76.15119298917683466 ) ) ;
#12749 = DIRECTION ( 'NONE',  ( 0.3895766659341561300, -0.003071955182676040438, 0.9209889165733659011 ) ) ;
#12750 = CARTESIAN_POINT ( 'NONE',  ( -1.477846259693492037, 50.16218137147969713, 69.15433879953098995 ) ) ;
#12751 = CARTESIAN_POINT ( 'NONE',  ( -0.2786462761171127345, 52.21223977499909807, 79.40856224512604911 ) ) ;
#12752 = DIRECTION ( 'NONE',  ( -1.540237394707284220E-16, -1.793354297423764243E-16, 1.000000000000000000 ) ) ;
#12753 = PLANE ( 'NONE',  #3467 ) ;
#12754 = CARTESIAN_POINT ( 'NONE',  ( 5.694198211105373275, 51.28221506855305734, 75.97344461144770378 ) ) ;
#12755 = CARTESIAN_POINT ( 'NONE',  ( 6.108721190857805183, 50.06200863618597197, 77.68963291717794561 ) ) ;
#12756 = ORIENTED_EDGE ( 'NONE', *, *, #4617, .T. ) ;
#12757 = ORIENTED_EDGE ( 'NONE', *, *, #17142, .F. ) ;
#12758 = EDGE_CURVE ( 'NONE', #5281, #15280, #16714, .T. ) ;
#12759 = DIRECTION ( 'NONE',  ( -1.402518428993831183E-16, 1.000000000000000000, -3.469446951953617640E-16 ) ) ;
#12761 = EDGE_CURVE ( 'NONE', #4049, #8055, #16204, .T. ) ;
#12760 = CARTESIAN_POINT ( 'NONE',  ( -4.199287694144524963, 50.86673310655319113, 75.97336489801017478 ) ) ;
#12762 = CARTESIAN_POINT ( 'NONE',  ( -4.831226022076290150, 37.17609274966823563, 78.89646723195187406 ) ) ;
#12763 = B_SPLINE_SURFACE_WITH_KNOTS ( 'NONE', 3, 1, ( 
 ( #710, #18580 ),
 ( #13693, #18798 ),
 ( #3996, #10836 ),
 ( #5922, #10414 ),
 ( #12419, #20490 ),
 ( #5597, #2621 ),
 ( #16882, #12317 ),
 ( #13894, #18898 ),
 ( #2416, #16983 ),
 ( #15610, #917 ),
 ( #1026, #7406 ),
 ( #4310, #12204 ),
 ( #10736, #20059 ),
 ( #817, #17199 ),
 ( #7518, #14006 ),
 ( #20378, #18477 ),
 ( #18684, #8914 ),
 ( #3893, #8800 ),
 ( #2303, #17301 ),
 ( #15292, #5696 ),
 ( #2726, #9231 ),
 ( #15404, #4102 ),
 ( #7301, #15504 ),
 ( #7190, #15718 ),
 ( #12103, #20167 ),
 ( #1137, #9019 ),
 ( #7625, #20266 ) ),
 .UNSPECIFIED., .F., .F., .F.,
 ( 4, 1, 1, 1, 1, 1, 1, 1, 1, 1, 1, 1, 1, 1, 1, 1, 1, 1, 1, 1, 1, 1, 1, 1, 4 ),
 ( 2, 2 ),
 ( 0.000000000000000000, 0.06065359464870424822, 0.1186516444374059315, 0.1737719091481386702, 0.2263851634537537849, 0.2765697945827291226, 0.3242346565764495647, 0.3697019794926615921, 0.4132083501371872081, 0.4544918499020897396, 0.4940385985015171566, 0.5318644461502587406, 0.5683353705239246878, 0.6034301395582813976, 0.6379278300831724424, 0.6713730032816831450, 0.7045442076430231682, 0.7379120707191915152, 0.7717275693920926383, 0.8063464942012584791, 0.8421824305429153057, 0.8795242022246468894, 0.9178549694745260501, 0.9579765912138670236, 1.000000000000000000 ),
 ( 0.000000000000000000, 1.000000000000000000 ),
 .UNSPECIFIED. ) ;
#12764 = CARTESIAN_POINT ( 'NONE',  ( 5.709672981839667649, 51.27078447877342882, 77.95044976498417100 ) ) ;
#12765 = CARTESIAN_POINT ( 'NONE',  ( 6.786106954071964736, 50.47566606489075980, 77.50555814853646552 ) ) ;
#12766 = CARTESIAN_POINT ( 'NONE',  ( -1.477846259693506470, 47.62628298661743997, 82.55433879953099563 ) ) ;
#12767 = DIRECTION ( 'NONE',  ( 0.007885122365275663500, 0.9999689119394085113, 1.805443505845543142E-16 ) ) ;
#12768 = EDGE_CURVE ( 'NONE', #3115, #972, #4523, .T. ) ;
#12769 = ADVANCED_FACE ( 'NONE', ( #19111 ), #6985, .T. ) ;
#12770 = ORIENTED_EDGE ( 'NONE', *, *, #3312, .T. ) ;
#12771 = CARTESIAN_POINT ( 'NONE',  ( -5.356359482101716196, 38.49999417901607757, 79.21211992218960063 ) ) ;
#12772 = FACE_OUTER_BOUND ( 'NONE', #19948, .T. ) ;
#12773 = PLANE ( 'NONE',  #15688 ) ;
#12774 = ORIENTED_EDGE ( 'NONE', *, *, #14712, .F. ) ;
#12775 = CARTESIAN_POINT ( 'NONE',  ( 23.29010293273768539, 19.08282756897896704, 45.55433879953098852 ) ) ;
#12776 = CARTESIAN_POINT ( 'NONE',  ( 4.001626195812781006, 40.29782224849783745, 89.72723091094957226 ) ) ;
#12777 = VERTEX_POINT ( 'NONE', #15722 ) ;
#12778 = CARTESIAN_POINT ( 'NONE',  ( -0.5941502889447408675, 52.21674969029312052, 75.69129100417544009 ) ) ;
#12779 = CARTESIAN_POINT ( 'NONE',  ( 8.292258355465955688, 41.60100403556243975, 78.05744560429982926 ) ) ;
#12780 = CARTESIAN_POINT ( 'NONE',  ( 5.611902828867023629, 37.90313308730407726, 78.37121987722640881 ) ) ;
#12781 = CARTESIAN_POINT ( 'NONE',  ( 0.8409237682492959332, 52.96364229810927071, 76.13704228601427815 ) ) ;
#12782 = CARTESIAN_POINT ( 'NONE',  ( 4.476015245556088651, 47.52441691994293649, 92.45433879953091605 ) ) ;
#12783 = ORIENTED_EDGE ( 'NONE', *, *, #1153, .F. ) ;
#12784 = DIRECTION ( 'NONE',  ( 1.000000000000000000, -1.110223024625156417E-16, -1.111814006898795283E-16 ) ) ;
#12785 = ORIENTED_EDGE ( 'NONE', *, *, #19352, .F. ) ;
#12786 = LINE ( 'NONE', #7896, #4008 ) ;
#12787 = EDGE_CURVE ( 'NONE', #374, #16250, #6226, .T. ) ;
#12788 = FACE_OUTER_BOUND ( 'NONE', #17491, .T. ) ;
#12789 = CARTESIAN_POINT ( 'NONE',  ( 31.22215374030650281, 42.76218137147968434, 78.80433879953099563 ) ) ;
#12790 = CARTESIAN_POINT ( 'NONE',  ( 4.921111604934655048, 46.69516597009693726, 95.01862182907727572 ) ) ;
#12791 = CARTESIAN_POINT ( 'NONE',  ( -6.427915807670530945, 42.26053564693651055, 78.13669174070733447 ) ) ;
#12792 = ORIENTED_EDGE ( 'NONE', *, *, #18972, .T. ) ;
#12793 = CARTESIAN_POINT ( 'NONE',  ( 34.76745320192723199, 38.96218137147968719, 93.55433879953098142 ) ) ;
#12794 = ORIENTED_EDGE ( 'NONE', *, *, #494, .F. ) ;
#12795 = VECTOR ( 'NONE', #14376, 1000.000000000000114 ) ;
#12796 = CARTESIAN_POINT ( 'NONE',  ( -3.704223681964030845, 51.95793902061026870, 75.61719165653033770 ) ) ;
#12797 = CARTESIAN_POINT ( 'NONE',  ( 6.828503391016846891, 43.33193468930419101, 94.16433880123797451 ) ) ;
#12798 = CARTESIAN_POINT ( 'NONE',  ( -7.785180019746818836, 41.22672913468994693, 78.61536821129558916 ) ) ;
#12799 = VERTEX_POINT ( 'NONE', #19204 ) ;
#12800 = CARTESIAN_POINT ( 'NONE',  ( -5.326399992380450144, 49.87884422129010886, 78.87652712212219797 ) ) ;
#12801 = CARTESIAN_POINT ( 'NONE',  ( 8.951667845840693971, 41.62244091939069790, 78.41904468188381827 ) ) ;
#12802 = CARTESIAN_POINT ( 'NONE',  ( -4.199131210323472807, 37.46382571656145899, 78.86760481232144571 ) ) ;
#12803 = EDGE_CURVE ( 'NONE', #18002, #13369, #17610, .T. ) ;
#12804 = CARTESIAN_POINT ( 'NONE',  ( 5.200841308562122123, 50.89200199683061498, 76.36928804473561172 ) ) ;
#12805 = LINE ( 'NONE', #1853, #761 ) ;
#12806 = ORIENTED_EDGE ( 'NONE', *, *, #14446, .F. ) ;
#12807 = CARTESIAN_POINT ( 'NONE',  ( -4.630511887643872448, 41.91479704223051783, 92.55433879953096721 ) ) ;
#12808 = CARTESIAN_POINT ( 'NONE',  ( 31.22215374030650281, 45.56218137147968861, 72.80433879953100984 ) ) ;
#12809 = ORIENTED_EDGE ( 'NONE', *, *, #6382, .F. ) ;
#12810 = CARTESIAN_POINT ( 'NONE',  ( 4.837856207073459203, 51.91476041137136832, 77.79664654212120922 ) ) ;
#12811 = DIRECTION ( 'NONE',  ( -1.540237394707284220E-16, -1.793354297423764243E-16, 1.000000000000000000 ) ) ;
#12812 = CARTESIAN_POINT ( 'NONE',  ( -5.831867965436852153, 50.43760231366965030, 76.45423404125398292 ) ) ;
#12813 = CARTESIAN_POINT ( 'NONE',  ( -1.876873622437039257, 39.01745058958429269, 92.87621379782399345 ) ) ;
#12814 = VECTOR ( 'NONE', #11514, 1000.000000000000114 ) ;
#12815 = CARTESIAN_POINT ( 'NONE',  ( 0.5221537403065118488, 48.16218137147969003, 45.55433879953100273 ) ) ;
#12816 = DIRECTION ( 'NONE',  ( 0.000000000000000000, -2.891205793294680792E-16, -1.000000000000000000 ) ) ;
#12817 = CARTESIAN_POINT ( 'NONE',  ( 5.560944854430392326, 50.62600801335337053, 76.13071926429850578 ) ) ;
#12818 = VERTEX_POINT ( 'NONE', #11249 ) ;
#12819 = CARTESIAN_POINT ( 'NONE',  ( -7.143058794816434798, 47.07503762047384299, 78.14998754261981162 ) ) ;
#12820 = EDGE_CURVE ( 'NONE', #11113, #16604, #14109, .T. ) ;
#12821 = VECTOR ( 'NONE', #17991, 1000.000000000000114 ) ;
#12822 = ORIENTED_EDGE ( 'NONE', *, *, #16270, .F. ) ;
#12823 = CARTESIAN_POINT ( 'NONE',  ( -7.852872584391570321, 41.45951414001282842, 78.01861101995372394 ) ) ;
#12824 = CARTESIAN_POINT ( 'NONE',  ( 5.448219197780140632, 37.61331060731148312, 77.67950998295866327 ) ) ;
#12825 = CARTESIAN_POINT ( 'NONE',  ( 28.52215374030649642, 40.96218137147970850, 87.05433879953100984 ) ) ;
#12826 = LINE ( 'NONE', #4526, #14583 ) ;
#12827 = ORIENTED_EDGE ( 'NONE', *, *, #7724, .F. ) ;
#12828 = CARTESIAN_POINT ( 'NONE',  ( 8.530649028577993676, 48.02340768410154936, 78.56977997600147035 ) ) ;
#12829 = VERTEX_POINT ( 'NONE', #9654 ) ;
#12830 = AXIS2_PLACEMENT_3D ( 'NONE', #20702, #18913, #14022 ) ;
#12831 = CARTESIAN_POINT ( 'NONE',  ( -3.196673508984729128, 36.89354759902561653, 75.82994300095940332 ) ) ;
#12832 = CARTESIAN_POINT ( 'NONE',  ( -4.161402579748598285, 37.43595709695774332, 76.29203488853940485 ) ) ;
#12833 = CARTESIAN_POINT ( 'NONE',  ( -5.058133621542618030, 44.89684013992257405, 93.92996379953099506 ) ) ;
#12834 = ORIENTED_EDGE ( 'NONE', *, *, #11554, .T. ) ;
#12835 = CARTESIAN_POINT ( 'NONE',  ( -4.585830261548859532, 37.76958990528607529, 77.32892190166411694 ) ) ;
#12836 =( BOUNDED_CURVE ( )  B_SPLINE_CURVE ( 3, ( #5286, #8616, #9790, #3695 ),
 .UNSPECIFIED., .F., .F. ) 
 B_SPLINE_CURVE_WITH_KNOTS ( ( 4, 4 ),
 ( 4.188790204786389637, 4.300872134317204498 ),
 .UNSPECIFIED. ) 
 CURVE ( )  GEOMETRIC_REPRESENTATION_ITEM ( )  RATIONAL_B_SPLINE_CURVE ( ( 1.000000000000000000, 0.9989534107080366709, 0.9989534107080366709, 1.000000000000000000 ) ) 
 REPRESENTATION_ITEM ( '' )  );
#12837 = CARTESIAN_POINT ( 'NONE',  ( 8.256691324932248222, 41.45960787672780157, 77.50846324053436831 ) ) ;
#12838 = CARTESIAN_POINT ( 'NONE',  ( 5.928963754087451576, 43.92611494815086814, 93.96996379953098710 ) ) ;
#12839 = EDGE_CURVE ( 'NONE', #11295, #14257, #19749, .T. ) ;
#12840 = ADVANCED_FACE ( 'NONE', ( #19414 ), #6747, .F. ) ;
#12841 = VERTEX_POINT ( 'NONE', #3251 ) ;
#12842 = CARTESIAN_POINT ( 'NONE',  ( 8.317158657711994252, 46.70735294479731436, 78.73595644658969661 ) ) ;
#12843 = DIRECTION ( 'NONE',  ( -1.110223024625156540E-16, -1.000000000000000000, -5.922860397471808077E-17 ) ) ;
#12844 = CARTESIAN_POINT ( 'NONE',  ( -5.427705199025447236, 38.51945526935772790, 79.11457076817336542 ) ) ;
#12845 = CARTESIAN_POINT ( 'NONE',  ( -4.524181921268124462, 40.28999182795290324, 91.19558880123797451 ) ) ;
#12846 = AXIS2_PLACEMENT_3D ( 'NONE', #15149, #12068, #15572 ) ;
#12847 =( NAMED_UNIT ( * ) PLANE_ANGLE_UNIT ( ) SI_UNIT ( $, .RADIAN. ) );
#12848 = CARTESIAN_POINT ( 'NONE',  ( 4.613683985508550300, 40.84891963687440608, 89.75946567728124137 ) ) ;
#12849 = CARTESIAN_POINT ( 'NONE',  ( 8.788263343888127466, 41.13270726085054463, 77.24417474779077963 ) ) ;
#12850 = CARTESIAN_POINT ( 'NONE',  ( 0.5221537403065061866, 44.16218137147969713, 74.55433879953100984 ) ) ;
#12851 = CARTESIAN_POINT ( 'NONE',  ( -0.7161872237684476783, 52.97813067712484525, 79.09854784679095019 ) ) ;
#12852 = ORIENTED_EDGE ( 'NONE', *, *, #4123, .F. ) ;
#12853 = CARTESIAN_POINT ( 'NONE',  ( -1.077846259693492126, 50.16218137147969713, 53.55433879953100273 ) ) ;
#12854 = CARTESIAN_POINT ( 'NONE',  ( 9.348773431696422165, 42.81259155210894107, 76.30013550906805619 ) ) ;
#12855 = CARTESIAN_POINT ( 'NONE',  ( 0.8409531834210948187, 52.35598196211776667, 76.19861658564380491 ) ) ;
#12856 = CARTESIAN_POINT ( 'NONE',  ( 2.392664886727894125, 47.70104341108812918, 53.28382765310963265 ) ) ;
#12857 = VECTOR ( 'NONE', #10615, 1000.000000000000000 ) ;
#12858 = VERTEX_POINT ( 'NONE', #19620 ) ;
#12859 = ADVANCED_FACE ( 'NONE', ( #6852 ), #5146, .F. ) ;
#12860 = CARTESIAN_POINT ( 'NONE',  ( 9.348773431696422165, 42.81259155210894107, 76.30013550906805619 ) ) ;
#12861 = CARTESIAN_POINT ( 'NONE',  ( -1.483269432489140005, 51.49895708687498086, 72.45433879953087342 ) ) ;
#12862 = CARTESIAN_POINT ( 'NONE',  ( -1.183761187420877548, 49.81017696809242068, 95.05433879953098142 ) ) ;
#12863 = CARTESIAN_POINT ( 'NONE',  ( 4.480833922618288945, 51.34373684881791178, 79.31790653140825498 ) ) ;
#12864 = CARTESIAN_POINT ( 'NONE',  ( -5.356086414478568258, 43.71529702833873898, 92.51086634196040848 ) ) ;
#12865 = CARTESIAN_POINT ( 'NONE',  ( -4.598246518171406727, 51.31910303412164609, 78.93669174070734584 ) ) ;
#12866 = FACE_OUTER_BOUND ( 'NONE', #6549, .T. ) ;
#12867 = CARTESIAN_POINT ( 'NONE',  ( 6.386126596379389397, 49.84628249594006633, 77.45110917081549928 ) ) ;
#12868 = CARTESIAN_POINT ( 'NONE',  ( 5.665287683258889651, 37.02150436742986273, 75.36022115247205022 ) ) ;
#12869 = CARTESIAN_POINT ( 'NONE',  ( 6.519924314245371555, 49.74745151145329203, 76.63889762306028786 ) ) ;
#12870 = AXIS2_PLACEMENT_3D ( 'NONE', #7595, #10905, #20652 ) ;
#12871 = EDGE_LOOP ( 'NONE', ( #7519, #13211, #15303, #2241 ) ) ;
#12872 = DIRECTION ( 'NONE',  ( 1.084202172485505420E-16, 1.000000000000000000, 0.000000000000000000 ) ) ;
#12873 = EDGE_CURVE ( 'NONE', #1135, #1015, #17990, .T. ) ;
#12874 = LINE ( 'NONE', #18188, #14309 ) ;
#12875 = EDGE_CURVE ( 'NONE', #16992, #9334, #6641, .T. ) ;
#12876 = CARTESIAN_POINT ( 'NONE',  ( 5.257910441395027945, 50.85640482246301275, 78.82166709644059210 ) ) ;
#12877 = DIRECTION ( 'NONE',  ( -1.000000000000000000, -1.402518428993831676E-16, -0.000000000000000000 ) ) ;
#12878 = EDGE_CURVE ( 'NONE', #9181, #12515, #16654, .T. ) ;
#12879 = EDGE_CURVE ( 'NONE', #10143, #983, #11666, .T. ) ;
#12880 = CARTESIAN_POINT ( 'NONE',  ( 8.810541937945364666, 41.19947762056773399, 75.36738766396204880 ) ) ;
#12881 = ORIENTED_EDGE ( 'NONE', *, *, #8497, .F. ) ;
#12882 = AXIS2_PLACEMENT_3D ( 'NONE', #3223, #13117, #19701 ) ;
#12883 = CARTESIAN_POINT ( 'NONE',  ( 6.447652509444688818, 38.50032921029611543, 76.69330938776616335 ) ) ;
#12884 = LINE ( 'NONE', #1918, #6070 ) ;
#12885 = CARTESIAN_POINT ( 'NONE',  ( 6.799065290779627624, 37.83166033551658103, 77.90902863000688683 ) ) ;
#12886 = DIRECTION ( 'NONE',  ( -0.4472135954999562069, 0.7745966692414842925, -0.4472135954999583718 ) ) ;
#12887 = ORIENTED_EDGE ( 'NONE', *, *, #6356, .F. ) ;
#12888 = CARTESIAN_POINT ( 'NONE',  ( -4.451527680475927617, 51.42394294381934117, 78.89116106075270807 ) ) ;
#12889 =( GEOMETRIC_REPRESENTATION_CONTEXT ( 3 ) GLOBAL_UNCERTAINTY_ASSIGNED_CONTEXT ( ( #5318 ) ) GLOBAL_UNIT_ASSIGNED_CONTEXT ( ( #2326, #2440, #7542 ) ) REPRESENTATION_CONTEXT ( 'NONE', 'WORKASPACE' ) );
#12890 = ORIENTED_EDGE ( 'NONE', *, *, #12741, .F. ) ;
#12891 = CARTESIAN_POINT ( 'NONE',  ( -0.9988176903691428077, 49.83852402762217082, 94.39871380123798872 ) ) ;
#12892 = VECTOR ( 'NONE', #5049, 1000.000000000000000 ) ;
#12893 = B_SPLINE_CURVE_WITH_KNOTS ( 'NONE', 3,
 ( #16810, #16705, #7217, #1627, #12032, #4902, #3705, #419, #8111, #3219, #6504, #11423, #9721, #13717, #18505 ),
 .UNSPECIFIED., .F., .F.,
 ( 4, 1, 1, 1, 1, 1, 1, 1, 1, 1, 1, 1, 4 ),
 ( 0.000000000000000000, 0.09897586389363323411, 0.1834007553115765132, 0.2562582723958196640, 0.3272804813821422187, 0.3687296102942994591, 0.4216358900696890455, 0.4870080516106923274, 0.5645314195351998077, 0.6541098812875514312, 0.7570203673134348055, 0.8723000540617986687, 1.000000000000000000 ),
 .UNSPECIFIED. ) ;
#12894 = CARTESIAN_POINT ( 'NONE',  ( 3.460444912181559474, 49.25145096859824889, 91.74246380123798872 ) ) ;
#12895 = CARTESIAN_POINT ( 'NONE',  ( 0.3411207544655743829, 52.36018373693247696, 76.11020748613105980 ) ) ;
#12896 = LINE ( 'NONE', #11208, #14064 ) ;
#12897 = DIRECTION ( 'NONE',  ( 1.000000000000000000, 1.402518428993842277E-16, 3.154042683594179442E-15 ) ) ;
#12898 = CIRCLE ( 'NONE', #9176, 8.800000000000000711 ) ;
#12899 = B_SPLINE_CURVE_WITH_KNOTS ( 'NONE', 3,
 ( #17888, #6600, #7898, #20755, #6189, #12895, #12693, #19377, #19171, #9716, #11521, #11107, #14386, #1621 ),
 .UNSPECIFIED., .F., .F.,
 ( 4, 2, 2, 2, 2, 2, 4 ),
 ( 0.000000000000000000, 0.0001566768555925129511, 0.0003133537111850259022, 0.0003916921389812823913, 0.0004700305667775389346, 0.0005483689945737954237, 0.0006267074223700516960 ),
 .UNSPECIFIED. ) ;
#12900 = ORIENTED_EDGE ( 'NONE', *, *, #13272, .T. ) ;
#12901 = DIRECTION ( 'NONE',  ( 0.9534635866061492715, 0.3015081906286096181, 2.009271279954798787E-16 ) ) ;
#12902 = ORIENTED_EDGE ( 'NONE', *, *, #7514, .F. ) ;
#12903 = VECTOR ( 'NONE', #17059, 1000.000000000000000 ) ;
#12904 = PLANE ( 'NONE',  #17341 ) ;
#12905 = AXIS2_PLACEMENT_3D ( 'NONE', #6733, #10055, #1955 ) ;
#12906 = EDGE_CURVE ( 'NONE', #17907, #14373, #18143, .T. ) ;
#12907 = CARTESIAN_POINT ( 'NONE',  ( 2.527576913102088874, 36.82540565608437078, 72.45432679953087529 ) ) ;
#12908 = CARTESIAN_POINT ( 'NONE',  ( -5.154188915835984375, 42.64120994080404614, 94.71121380123797451 ) ) ;
#12909 = ORIENTED_EDGE ( 'NONE', *, *, #20743, .F. ) ;
#12910 = CARTESIAN_POINT ( 'NONE',  ( -5.286500981006134303, 49.90735459402215213, 78.97495844722888592 ) ) ;
#12911 = CARTESIAN_POINT ( 'NONE',  ( -5.606854386412797098, 37.74901817818727778, 79.39214668191834789 ) ) ;
#12912 = CARTESIAN_POINT ( 'NONE',  ( -4.661432690376161148, 37.05067325523394572, 78.93441095796421791 ) ) ;
#12913 = CARTESIAN_POINT ( 'NONE',  ( 5.600448134661695221, 51.35146447353857013, 76.04240903267428564 ) ) ;
#12914 = CARTESIAN_POINT ( 'NONE',  ( 2.580190882731753010, 49.45805475339454205, 93.29925044102854770 ) ) ;
#12915 = ORIENTED_EDGE ( 'NONE', *, *, #13855, .T. ) ;
#12916 = VECTOR ( 'NONE', #3524, 1000.000000000000114 ) ;
#12917 = CARTESIAN_POINT ( 'NONE',  ( -2.077846259693550746, 39.65884927180063357, 92.91433879953098085 ) ) ;
#12918 = VECTOR ( 'NONE', #446, 1000.000000000000000 ) ;
#12919 = PLANE ( 'NONE',  #4852 ) ;
#12920 = ORIENTED_EDGE ( 'NONE', *, *, #10583, .F. ) ;
#12921 = CARTESIAN_POINT ( 'NONE',  ( 4.248944230316001658, 51.43575096055252516, 77.94290914044947272 ) ) ;
#12922 = DIRECTION ( 'NONE',  ( 3.893792155548169402E-16, 7.183611964723547524E-17, -1.000000000000000000 ) ) ;
#12923 = CARTESIAN_POINT ( 'NONE',  ( 0.6357006819926122043, 52.96147595994789015, 78.93320643228391020 ) ) ;
#12924 = CARTESIAN_POINT ( 'NONE',  ( 0.2860873169776699254, 38.75537135769874197, 94.59496379611701400 ) ) ;
#12925 = VECTOR ( 'NONE', #18090, 1000.000000000000000 ) ;
#12926 = CARTESIAN_POINT ( 'NONE',  ( 0.5221537403065056315, 44.16218137147969713, 77.55433879953099563 ) ) ;
#12927 = DIRECTION ( 'NONE',  ( -1.000000000000000000, 0.000000000000000000, 0.000000000000000000 ) ) ;
#12928 = CARTESIAN_POINT ( 'NONE',  ( 5.266681877975375237, 37.48359068508447933, 77.75986257808632729 ) ) ;
#12929 = LINE ( 'NONE', #11348, #18767 ) ;
#12930 = ORIENTED_EDGE ( 'NONE', *, *, #2356, .T. ) ;
#12931 = CARTESIAN_POINT ( 'NONE',  ( 2.002786569115004855, 52.95507841157613171, 78.99734963310253022 ) ) ;
#12932 = AXIS2_PLACEMENT_3D ( 'NONE', #8593, #11473, #13164 ) ;
#12933 = EDGE_LOOP ( 'NONE', ( #9822, #8430, #7626, #17320, #2831 ) ) ;
#12934 = CARTESIAN_POINT ( 'NONE',  ( 6.722153740306509917, 44.16218137147969003, 111.0905869729573681 ) ) ;
#12935 = CARTESIAN_POINT ( 'NONE',  ( 0.5221537403065085181, 49.16218137147969003, 93.04136871766880290 ) ) ;
#12936 = LINE ( 'NONE', #3153, #20762 ) ;
#12937 = B_SPLINE_SURFACE_WITH_KNOTS ( 'NONE', 3, 1, ( 
 ( #17620, #7848 ),
 ( #4846, #20809 ),
 ( #16044, #3263 ),
 ( #9762, #8154 ),
 ( #3572, #5363 ),
 ( #13157, #171 ),
 ( #11572, #8264 ),
 ( #19838, #5258 ),
 ( #10077, #11677 ),
 ( #375, #11876 ),
 ( #18356, #3776 ),
 ( #11469, #1784 ),
 ( #13464, #9979 ),
 ( #3470, #72 ),
 ( #14644, #18047 ),
 ( #11774, #8369 ),
 ( #481, #18250 ),
 ( #10294, #14750 ),
 ( #6551, #16460 ) ),
 .UNSPECIFIED., .F., .F., .F.,
 ( 4, 1, 1, 1, 1, 1, 1, 1, 1, 1, 1, 1, 1, 1, 1, 1, 4 ),
 ( 2, 2 ),
 ( 0.000000000000000000, 0.1026547437176949656, 0.1953110930976798554, 0.2773242249590897601, 0.3493914542831295655, 0.4108068724308638342, 0.4622887491528899773, 0.5032980238437735343, 0.5345418472720404601, 0.5847168530758872773, 0.6322731508218554231, 0.6775315938118185999, 0.7246750034944897667, 0.7779009386454487363, 0.8408031781967141294, 0.9146367246678260843, 1.000000000000000000 ),
 ( 0.000000000000000000, 1.000000000000000000 ),
 .UNSPECIFIED. ) ;
#12938 = CARTESIAN_POINT ( 'NONE',  ( 8.744145067270602922, 41.00048198701652780, 79.52393066155629242 ) ) ;
#12939 = ORIENTED_EDGE ( 'NONE', *, *, #6156, .F. ) ;
#12940 = CARTESIAN_POINT ( 'NONE',  ( 5.939900590116411472, 51.10072461867315496, 76.90580938776616904 ) ) ;
#12941 = CARTESIAN_POINT ( 'NONE',  ( -7.184859864745180680, 41.78596111121809997, 79.54845644658969661 ) ) ;
#12942 = ORIENTED_EDGE ( 'NONE', *, *, #7658, .F. ) ;
#12943 = VECTOR ( 'NONE', #8626, 1000.000000000000000 ) ;
#12944 = CARTESIAN_POINT ( 'NONE',  ( 5.677877744449962627, 51.29427033984291029, 78.92241520643889885 ) ) ;
#12945 = LINE ( 'NONE', #15932, #11888 ) ;
#12946 = VERTEX_POINT ( 'NONE', #12935 ) ;
#12947 = CARTESIAN_POINT ( 'NONE',  ( -1.677846259693485109, 49.95873206995546667, 56.15433879953099705 ) ) ;
#12948 = CARTESIAN_POINT ( 'NONE',  ( 8.787829143201870252, 41.13140593384865440, 77.14698585835439815 ) ) ;
#12949 = CARTESIAN_POINT ( 'NONE',  ( 0.7901638384306286511, 50.30062182352762079, 92.17308879782397923 ) ) ;
#12950 = VERTEX_POINT ( 'NONE', #9857 ) ;
#12951 = CARTESIAN_POINT ( 'NONE',  ( -4.804516487068378083, 51.17171006637344277, 76.41659450085566618 ) ) ;
#12952 = LINE ( 'NONE', #19433, #4069 ) ;
#12953 = EDGE_CURVE ( 'NONE', #10926, #4092, #9751, .T. ) ;
#12954 = UNCERTAINTY_MEASURE_WITH_UNIT (LENGTH_MEASURE( 1.000000000000000082E-05 ), #6145, 'distance_accuracy_value', 'NONE');
#12955 = CARTESIAN_POINT ( 'NONE',  ( -5.644616003178662744, 50.57140571016744701, 75.79002994479621691 ) ) ;
#12956 = CARTESIAN_POINT ( 'NONE',  ( 8.951667845840693971, 41.62244091939069790, 76.38301527011910252 ) ) ;
#12957 = DIRECTION ( 'NONE',  ( -1.779391786395883536E-16, -5.922860397471806844E-17, 1.000000000000000000 ) ) ;
#12958 = CARTESIAN_POINT ( 'NONE',  ( 8.648170029844118645, 43.06315486489794608, 76.74257409364851412 ) ) ;
#12959 = ORIENTED_EDGE ( 'NONE', *, *, #8592, .F. ) ;
#12960 = AXIS2_PLACEMENT_3D ( 'NONE', #10635, #18801, #4214 ) ;
#12961 = CARTESIAN_POINT ( 'NONE',  ( -0.4699484075729998822, 52.36218137147968577, 83.03825919817350609 ) ) ;
#12962 = CARTESIAN_POINT ( 'NONE',  ( 8.317158657711994252, 46.70735294479731436, 78.73595644658969661 ) ) ;
#12963 = PLANE ( 'NONE',  #20759 ) ;
#12964 = CARTESIAN_POINT ( 'NONE',  ( -1.477846259693489150, 50.16218137147969713, 53.55433879953100273 ) ) ;
#12965 = VECTOR ( 'NONE', #9593, 1000.000000000000000 ) ;
#12966 =( BOUNDED_CURVE ( )  B_SPLINE_CURVE ( 3, ( #4987, #1823, #14579, #11509 ),
 .UNSPECIFIED., .F., .F. ) 
 B_SPLINE_CURVE_WITH_KNOTS ( ( 4, 4 ),
 ( 5.006904465492823419, 5.052225889838807937 ),
 .UNSPECIFIED. ) 
 CURVE ( )  GEOMETRIC_REPRESENTATION_ITEM ( )  RATIONAL_B_SPLINE_CURVE ( ( 1.000000000000000000, 0.9998288380325438540, 0.9998288380325438540, 1.000000000000000000 ) ) 
 REPRESENTATION_ITEM ( '' )  );
#12967 = VERTEX_POINT ( 'NONE', #16342 ) ;
#12968 = ORIENTED_EDGE ( 'NONE', *, *, #14367, .T. ) ;
#12969 = CARTESIAN_POINT ( 'NONE',  ( 7.680032241523796266, 40.16158449578585277, 77.13595644658970230 ) ) ;
#12970 = CARTESIAN_POINT ( 'NONE',  ( 1.652727357819364640, 35.35299279957455809, 75.45433879953087342 ) ) ;
#12971 = CARTESIAN_POINT ( 'NONE',  ( -4.895593109503408868, 37.22363812428621088, 78.53742703482498655 ) ) ;
#12972 = EDGE_CURVE ( 'NONE', #15788, #15424, #2760, .T. ) ;
#12973 = DIRECTION ( 'NONE',  ( -1.111814006898795283E-16, 5.922860397471810542E-17, -1.000000000000000000 ) ) ;
#12974 = CARTESIAN_POINT ( 'NONE',  ( 5.666884522201895535, 41.76315400873614436, 93.03246379782397923 ) ) ;
#12975 = LINE ( 'NONE', #19455, #5002 ) ;
#12976 = EDGE_CURVE ( 'NONE', #7376, #6491, #20993, .T. ) ;
#12977 = CARTESIAN_POINT ( 'NONE',  ( -5.968382836370074607, 47.45797339585421071, 78.32492703482499508 ) ) ;
#12978 = VECTOR ( 'NONE', #7728, 1000.000000000000000 ) ;
#12979 = LINE ( 'NONE', #11395, #20054 ) ;
#12980 = DIRECTION ( 'NONE',  ( 0.000000000000000000, 2.891205793294680792E-16, 1.000000000000000000 ) ) ;
#12981 = CIRCLE ( 'NONE', #14676, 0.5999999999999928724 ) ;
#12982 = CARTESIAN_POINT ( 'NONE',  ( -0.9988176903691428077, 49.83852402762217082, 91.89871380123798872 ) ) ;
#12983 = ORIENTED_EDGE ( 'NONE', *, *, #652, .F. ) ;
#12984 = LINE ( 'NONE', #4877, #6130 ) ;
#12985 = EDGE_LOOP ( 'NONE', ( #916, #5536, #17931, #20684 ) ) ;
#12986 = ADVANCED_FACE ( 'NONE', ( #19828, #11456, #14632, #5249 ), #8358, .F. ) ;
#12987 = CARTESIAN_POINT ( 'NONE',  ( 8.946998292058729874, 41.60844597047518789, 78.80177617112552468 ) ) ;
#12988 = CARTESIAN_POINT ( 'NONE',  ( -3.219615297498348738, 36.86557920496366592, 77.48809274675903680 ) ) ;
#12989 = AXIS2_PLACEMENT_3D ( 'NONE', #7298, #6014, #10734 ) ;
#12990 = CIRCLE ( 'NONE', #3479, 8.199999999999995737 ) ;
#12991 = CARTESIAN_POINT ( 'NONE',  ( 8.874399228141724549, 41.39086197031718228, 75.36031793586835192 ) ) ;
#12992 = ORIENTED_EDGE ( 'NONE', *, *, #14631, .F. ) ;
#12993 = CARTESIAN_POINT ( 'NONE',  ( 5.951216973768841179, 38.14559455216716799, 75.49608936836499140 ) ) ;
#12994 = CARTESIAN_POINT ( 'NONE',  ( 0.1818310095788190917, 52.97104947332776703, 79.52116152017964623 ) ) ;
#12995 = PLANE ( 'NONE',  #13815 ) ;
#12996 = CARTESIAN_POINT ( 'NONE',  ( -3.496029822981026491, 36.18983710238020279, 76.51650556680409920 ) ) ;
#12997 = DIRECTION ( 'NONE',  ( -0.3165065846431827645, -0.9485903129789529098, 0.000000000000000000 ) ) ;
#12998 = EDGE_CURVE ( 'NONE', #9835, #19503, #16234, .T. ) ;
#12999 = VERTEX_POINT ( 'NONE', #9969 ) ;
#13000 = EDGE_CURVE ( 'NONE', #19814, #9748, #8142, .T. ) ;
#13001 = CARTESIAN_POINT ( 'NONE',  ( -4.383473025373059606, 51.47257230871590394, 78.45066232894264147 ) ) ;
#13002 = ADVANCED_FACE ( 'NONE', ( #1969 ), #588, .T. ) ;
#13003 = ORIENTED_EDGE ( 'NONE', *, *, #17509, .T. ) ;
#13004 = CARTESIAN_POINT ( 'NONE',  ( -0.8237052942265477018, 49.18499566818285018, 95.25808880294498238 ) ) ;
#13005 = DIRECTION ( 'NONE',  ( -1.000000000000000000, -1.402518428993831676E-16, -1.196361017915039239E-16 ) ) ;
#13006 = AXIS2_PLACEMENT_3D ( 'NONE', #8292, #194, #3496 ) ;
#13007 = CARTESIAN_POINT ( 'NONE',  ( 5.844285037446443454, 37.14940932322087264, 76.26708001093082601 ) ) ;
#13008 = VECTOR ( 'NONE', #8517, 1000.000000000000114 ) ;
#13009 = CARTESIAN_POINT ( 'NONE',  ( -5.950833756536985319, 38.00310188256379007, 76.46818962967083166 ) ) ;
#13010 = ADVANCED_FACE ( 'NONE', ( #10344 ), #4804, .F. ) ;
#13011 = CARTESIAN_POINT ( 'NONE',  ( 0.8377421044266867289, 51.35991668224300355, 78.52566232894263010 ) ) ;
#13012 = VERTEX_POINT ( 'NONE', #17693 ) ;
#13013 = DIRECTION ( 'NONE',  ( -0.000000000000000000, -0.000000000000000000, 1.000000000000000000 ) ) ;
#13014 = ORIENTED_EDGE ( 'NONE', *, *, #17649, .F. ) ;
#13015 = CARTESIAN_POINT ( 'NONE',  ( 2.927603783594689091, 51.37146775011972011, 75.45433879953087342 ) ) ;
#13016 = CARTESIAN_POINT ( 'NONE',  ( -5.784195910403845176, 44.99242805365518194, 92.28933880123798872 ) ) ;
#13017 = CARTESIAN_POINT ( 'NONE',  ( 6.828503391016846891, 43.33193468930419101, 94.00808880123798872 ) ) ;
#13018 = VERTEX_POINT ( 'NONE', #4905 ) ;
#13019 = CARTESIAN_POINT ( 'NONE',  ( -5.403220070277449771, 49.82395140618747575, 78.14282209630749776 ) ) ;
#13020 = DIRECTION ( 'NONE',  ( -1.000000000000000000, -1.402518428993831676E-16, -0.000000000000000000 ) ) ;
#13021 = AXIS2_PLACEMENT_3D ( 'NONE', #5877, #4364, #871 ) ;
#13022 = CARTESIAN_POINT ( 'NONE',  ( 4.372497882239381184, 39.86211998552705893, 92.55433879953093879 ) ) ;
#13023 = DIRECTION ( 'NONE',  ( 1.000000000000000000, -0.000000000000000000, -0.000000000000000000 ) ) ;
#13024 = FACE_OUTER_BOUND ( 'NONE', #1124, .T. ) ;
#13025 = VERTEX_POINT ( 'NONE', #8223 ) ;
#13026 = DIRECTION ( 'NONE',  ( -0.5813877811927010697, 0.8136266022444373913, 5.636455622144621648E-17 ) ) ;
#13027 = CARTESIAN_POINT ( 'NONE',  ( 0.5221537403065097394, 44.16218137147969003, 80.55433879953099563 ) ) ;
#13028 = ORIENTED_EDGE ( 'NONE', *, *, #8190, .T. ) ;
#13029 = CARTESIAN_POINT ( 'NONE',  ( -1.898293902487090401, 49.05989174320345114, 95.05433879953098142 ) ) ;
#13030 = EDGE_CURVE ( 'NONE', #19237, #10307, #11323, .T. ) ;
#13031 = CARTESIAN_POINT ( 'NONE',  ( -7.093231395208066559, 41.52507926682920214, 76.45513158819304067 ) ) ;
#13032 = CARTESIAN_POINT ( 'NONE',  ( -4.790713360849209401, 51.18157327500495768, 75.36324311589748959 ) ) ;
#13033 = CARTESIAN_POINT ( 'NONE',  ( 4.178421596892071044, 40.17206517740157778, 92.25121379611699979 ) ) ;
#13034 = CARTESIAN_POINT ( 'NONE',  ( -4.812088799398939187, 42.22067586467031930, 92.56371379782397923 ) ) ;
#13035 = EDGE_CURVE ( 'NONE', #12829, #3770, #5012, .T. ) ;
#13036 = PLANE ( 'NONE',  #11236 ) ;
#13037 = FACE_OUTER_BOUND ( 'NONE', #19525, .T. ) ;
#13038 = EDGE_CURVE ( 'NONE', #13701, #1661, #10658, .T. ) ;
#13039 = VECTOR ( 'NONE', #17646, 1000.000000000000000 ) ;
#13040 = CARTESIAN_POINT ( 'NONE',  ( -3.522017727535928344, 36.20903332061824642, 77.14704031750767399 ) ) ;
#13041 = ORIENTED_EDGE ( 'NONE', *, *, #18102, .F. ) ;
#13042 = PLANE ( 'NONE',  #11883 ) ;
#13043 = DIRECTION ( 'NONE',  ( 1.000000000000000000, 0.000000000000000000, 0.000000000000000000 ) ) ;
#13044 = VERTEX_POINT ( 'NONE', #13224 ) ;
#13045 = FACE_OUTER_BOUND ( 'NONE', #14590, .T. ) ;
#13046 = CARTESIAN_POINT ( 'NONE',  ( -1.392380047608626992, 49.84925249003584469, 85.23980501161585721 ) ) ;
#13047 = CARTESIAN_POINT ( 'NONE',  ( 8.887668352622405621, 41.43063037816333605, 75.36022115247205022 ) ) ;
#13048 = VERTEX_POINT ( 'NONE', #1846 ) ;
#13049 = CARTESIAN_POINT ( 'NONE',  ( 6.198496396448986090, 45.68315280215533392, 94.24246380123798872 ) ) ;
#13050 = CARTESIAN_POINT ( 'NONE',  ( -3.777846259693487418, 51.36218137147968577, 54.55433879953099563 ) ) ;
#13051 = VERTEX_POINT ( 'NONE', #18115 ) ;
#13052 = DIRECTION ( 'NONE',  ( 0.7071067811865515695, 0.7071067811865434649, 0.000000000000000000 ) ) ;
#13053 = DIRECTION ( 'NONE',  ( -0.5941461771851693774, -0.8043570849667760481, -2.357623395011396791E-16 ) ) ;
#13054 = CARTESIAN_POINT ( 'NONE',  ( -5.058133621542618030, 44.89684013992257405, 96.42996379953098085 ) ) ;
#13055 = VERTEX_POINT ( 'NONE', #11639 ) ;
#13056 = CARTESIAN_POINT ( 'NONE',  ( -4.316692190778365301, 37.57078845395070488, 77.27854074750605662 ) ) ;
#13057 = LINE ( 'NONE', #272, #14603 ) ;
#13058 = CARTESIAN_POINT ( 'NONE',  ( 2.232254456934870568, 39.46371826755015633, 94.98558879953097289 ) ) ;
#13059 = CIRCLE ( 'NONE', #4874, 4.200000000000000178 ) ;
#13060 = ORIENTED_EDGE ( 'NONE', *, *, #12121, .T. ) ;
#13061 = DIRECTION ( 'NONE',  ( -0.007885122365275663500, -0.9999689119394085113, -1.805443505845543142E-16 ) ) ;
#13062 = CARTESIAN_POINT ( 'NONE',  ( -1.174478664588463728, 57.66640723084523046, 80.55433879953099563 ) ) ;
#13063 = CARTESIAN_POINT ( 'NONE',  ( 6.828503391016846891, 43.33193468930419101, 94.00808880123798872 ) ) ;
#13064 = EDGE_CURVE ( 'NONE', #6327, #10505, #9940, .T. ) ;
#13065 = CARTESIAN_POINT ( 'NONE',  ( 6.817737414320570899, 50.45230191805777054, 75.81347835631012799 ) ) ;
#13066 = LINE ( 'NONE', #9569, #11649 ) ;
#13067 = CARTESIAN_POINT ( 'NONE',  ( 0.5221537403065015237, 44.16218137147968292, 75.45433879953088763 ) ) ;
#13068 = CARTESIAN_POINT ( 'NONE',  ( 8.479137094719348511, 40.20623628148813111, 79.16795596456493911 ) ) ;
#13069 = ORIENTED_EDGE ( 'NONE', *, *, #1917, .F. ) ;
#13070 = DIRECTION ( 'NONE',  ( -0.3165065846431827090, -0.9485903129789527988, 0.000000000000000000 ) ) ;
#13071 = CARTESIAN_POINT ( 'NONE',  ( 8.587085583998218752, 42.89418280249433479, 75.81656704941096336 ) ) ;
#13072 = DIRECTION ( 'NONE',  ( 0.000000000000000000, -3.469446951953617640E-16, -1.000000000000000000 ) ) ;
#13073 = CARTESIAN_POINT ( 'NONE',  ( 2.075677826575113016, 52.82397334471521333, 78.80921410649150971 ) ) ;
#13074 = EDGE_LOOP ( 'NONE', ( #3107, #20998, #6900, #2697 ) ) ;
#13075 = CARTESIAN_POINT ( 'NONE',  ( -1.219056181852248066, 49.77488197367201650, 94.56237966814981633 ) ) ;
#13076 = EDGE_LOOP ( 'NONE', ( #15956, #11525, #7812, #14889 ) ) ;
#13077 = B_SPLINE_CURVE_WITH_KNOTS ( 'NONE', 3,
 ( #14647, #1883, #11266, #174, #11471, #3364, #13161, #17737 ),
 .UNSPECIFIED., .F., .F.,
 ( 4, 2, 2, 4 ),
 ( 0.000000000000000000, 0.0001105466857480712239, 0.0002210933714961424478, 0.0004421867429922453222 ),
 .UNSPECIFIED. ) ;
#13078 = EDGE_CURVE ( 'NONE', #17279, #10129, #15218, .T. ) ;
#13079 = CARTESIAN_POINT ( 'NONE',  ( 7.698155637638221194, 40.19417714920118812, 76.18042117906708199 ) ) ;
#13080 = FACE_OUTER_BOUND ( 'NONE', #8310, .T. ) ;
#13081 = CARTESIAN_POINT ( 'NONE',  ( 1.119863296874943126, 50.25084051303456789, 61.06567965797611208 ) ) ;
#13082 = CARTESIAN_POINT ( 'NONE',  ( -1.047061061252479108, 36.11373028406117669, 75.45433879953087342 ) ) ;
#13083 = CARTESIAN_POINT ( 'NONE',  ( 0.2541436421823703995, 38.02374091943176637, 94.04808879782399345 ) ) ;
#13084 = CARTESIAN_POINT ( 'NONE',  ( 8.614432416951936844, 42.97614299570737018, 77.68070116889359156 ) ) ;
#13085 = PLANE ( 'NONE',  #12180 ) ;
#13086 = CARTESIAN_POINT ( 'NONE',  ( 5.722153740306476166, 44.16218185472587976, 94.89411094854372664 ) ) ;
#13087 = CARTESIAN_POINT ( 'NONE',  ( 6.828503391016846891, 43.33193468930419101, 90.25808880123800293 ) ) ;
#13088 = VERTEX_POINT ( 'NONE', #16105 ) ;
#13089 = DIRECTION ( 'NONE',  ( 1.402518428993831676E-16, -1.000000000000000000, 0.000000000000000000 ) ) ;
#13090 = CARTESIAN_POINT ( 'NONE',  ( -3.539401246598059991, 43.09270903039240608, 82.45433879953087342 ) ) ;
#13091 = CARTESIAN_POINT ( 'NONE',  ( 8.647984279038439581, 43.06178145482667219, 76.54298940512656202 ) ) ;
#13092 = EDGE_CURVE ( 'NONE', #4359, #10285, #4801, .T. ) ;
#13093 = LINE ( 'NONE', #11617, #10577 ) ;
#13094 = PLANE ( 'NONE',  #18992 ) ;
#13095 = VERTEX_POINT ( 'NONE', #20091 ) ;
#13096 = ORIENTED_EDGE ( 'NONE', *, *, #2519, .F. ) ;
#13097 = EDGE_CURVE ( 'NONE', #14733, #14867, #7192, .T. ) ;
#13098 = CARTESIAN_POINT ( 'NONE',  ( 6.859321636172213132, 37.87471731380851026, 76.18799845131768222 ) ) ;
#13099 = FACE_OUTER_BOUND ( 'NONE', #13672, .T. ) ;
#13100 = CARTESIAN_POINT ( 'NONE',  ( 8.224838919204344734, 41.34743166599955089, 79.54253259009090016 ) ) ;
#13101 = DIRECTION ( 'NONE',  ( -1.000000000000000000, -5.084437235940625660E-16, 0.000000000000000000 ) ) ;
#13102 = CARTESIAN_POINT ( 'NONE',  ( 5.389492195292208798, 36.82443100924615464, 78.09625056423675460 ) ) ;
#13103 = ORIENTED_EDGE ( 'NONE', *, *, #17085, .F. ) ;
#13104 = CARTESIAN_POINT ( 'NONE',  ( 14.52215374030650175, 40.36218137147969287, 105.5543387995309956 ) ) ;
#13105 = EDGE_CURVE ( 'NONE', #9723, #14881, #10619, .T. ) ;
#13106 = ORIENTED_EDGE ( 'NONE', *, *, #11540, .F. ) ;
#13107 = CARTESIAN_POINT ( 'NONE',  ( -2.416137431568557314, 39.07291177436112406, 91.11746380123798872 ) ) ;
#13108 = CARTESIAN_POINT ( 'NONE',  ( 1.338678443490884273, 52.94638778455286143, 76.79234737414994072 ) ) ;
#13109 = CARTESIAN_POINT ( 'NONE',  ( -3.096104608208455566, 36.80844346142616530, 78.46683879953087626 ) ) ;
#13110 = CARTESIAN_POINT ( 'NONE',  ( -7.373158828693091138, 41.96119617500171728, 78.52713215918005574 ) ) ;
#13111 = B_SPLINE_SURFACE_WITH_KNOTS ( 'NONE', 3, 1, ( 
 ( #17716, #9745 ),
 ( #15918, #18028 ),
 ( #1765, #16227 ),
 ( #5034, #13136 ),
 ( #9542, #19407 ),
 ( #9430, #1652 ),
 ( #19612, #12817 ),
 ( #9647, #11552 ),
 ( #8134, #1339 ),
 ( #11242, #20789 ),
 ( #6531, #4926 ),
 ( #3032, #11450 ),
 ( #17919, #3342 ),
 ( #9848, #14311 ),
 ( #7933, #14415 ) ),
 .UNSPECIFIED., .F., .F., .F.,
 ( 4, 1, 1, 1, 1, 1, 1, 1, 1, 1, 1, 1, 4 ),
 ( 2, 2 ),
 ( 0.000000000000000000, 0.1124872259413081665, 0.2145177594606929306, 0.3061691560909166610, 0.3877635431594634863, 0.4596729905988826692, 0.5233009716387192478, 0.5766443983521717387, 0.6225226080321302202, 0.7076769590374641927, 0.7964950891574525960, 0.8912003305064800651, 1.000000000000000000 ),
 ( 0.000000000000000000, 1.000000000000000000 ),
 .UNSPECIFIED. ) ;
#13112 = CARTESIAN_POINT ( 'NONE',  ( 8.648042534604279297, 43.06221218663710459, 78.51015103835841558 ) ) ;
#13113 = ORIENTED_EDGE ( 'NONE', *, *, #9485, .F. ) ;
#13114 = ORIENTED_EDGE ( 'NONE', *, *, #18211, .F. ) ;
#13115 = CARTESIAN_POINT ( 'NONE',  ( 0.5221537403065006355, 44.16218137147969003, 92.45433879953097289 ) ) ;
#13116 = CARTESIAN_POINT ( 'NONE',  ( 4.394343283833276992, 39.11584570990505938, 91.50808880123798872 ) ) ;
#13117 = DIRECTION ( 'NONE',  ( 1.540237394707284220E-16, 1.793354297423764243E-16, -1.000000000000000000 ) ) ;
#13118 = ORIENTED_EDGE ( 'NONE', *, *, #1680, .T. ) ;
#13119 = CARTESIAN_POINT ( 'NONE',  ( -5.668520211720758262, 50.55432463793220421, 79.06611278947218580 ) ) ;
#13120 = DIRECTION ( 'NONE',  ( -1.540237394707284220E-16, -1.793354297423764243E-16, 1.000000000000000000 ) ) ;
#13121 = CARTESIAN_POINT ( 'NONE',  ( 4.135038682601217097, 47.90320695352507130, 92.55433879953098142 ) ) ;
#13122 = DIRECTION ( 'NONE',  ( -0.3165065846431824870, -0.9485903129789529098, 0.000000000000000000 ) ) ;
#13123 = CARTESIAN_POINT ( 'NONE',  ( 5.076982970477778245, 37.34803879110698688, 77.55899030588862786 ) ) ;
#13124 = VERTEX_POINT ( 'NONE', #16913 ) ;
#13125 = FACE_OUTER_BOUND ( 'NONE', #434, .T. ) ;
#13126 = CARTESIAN_POINT ( 'NONE',  ( 0.8503869109451517305, 52.96349527369733323, 78.52566232894263010 ) ) ;
#13127 = ORIENTED_EDGE ( 'NONE', *, *, #15477, .F. ) ;
#13128 = CARTESIAN_POINT ( 'NONE',  ( 4.151429181450037476, 51.50778139900403119, 78.23954818826248925 ) ) ;
#13129 = CARTESIAN_POINT ( 'NONE',  ( -7.445240191484915115, 40.15417470793909871, 78.06261470525505786 ) ) ;
#13130 = CARTESIAN_POINT ( 'NONE',  ( -4.217603907031332255, 50.67132072554849742, 75.36022115247205022 ) ) ;
#13131 = CARTESIAN_POINT ( 'NONE',  ( 5.053692675489761754, 42.04909006277621586, 94.82933879611698558 ) ) ;
#13132 = CARTESIAN_POINT ( 'NONE',  ( 5.856396280011940902, 46.10368687828906076, 91.93871379782397923 ) ) ;
#13133 = DIRECTION ( 'NONE',  ( -1.540237394707284467E-16, -1.793354297423764243E-16, 1.000000000000000000 ) ) ;
#13134 = CARTESIAN_POINT ( 'NONE',  ( 0.5221537403065364957, 44.16218137147969003, 123.5543387995310098 ) ) ;
#13135 = VECTOR ( 'NONE', #14646, 1000.000000000000114 ) ;
#13136 = CARTESIAN_POINT ( 'NONE',  ( 5.576569238758990465, 50.61446691003841636, 76.26580079864017137 ) ) ;
#13137 = ORIENTED_EDGE ( 'NONE', *, *, #20758, .T. ) ;
#13138 = CARTESIAN_POINT ( 'NONE',  ( 1.647117196182025678, 52.95788299529235843, 79.33873778842219338 ) ) ;
#13139 = CARTESIAN_POINT ( 'NONE',  ( 5.160332980892567534, 37.41848089432694024, 78.21801395346943764 ) ) ;
#13140 = EDGE_CURVE ( 'NONE', #10043, #5117, #2657, .T. ) ;
#13141 = CARTESIAN_POINT ( 'NONE',  ( -3.704223681964030845, 51.95793902061026870, 75.61719165653033770 ) ) ;
#13142 = ORIENTED_EDGE ( 'NONE', *, *, #5940, .T. ) ;
#13143 = DIRECTION ( 'NONE',  ( 0.5813877811927011807, -0.8136266022444372803, -5.636455622144619183E-17 ) ) ;
#13144 = EDGE_CURVE ( 'NONE', #6239, #5759, #847, .T. ) ;
#13145 = CARTESIAN_POINT ( 'NONE',  ( 27.27315414062681853, 40.36218137147969287, 105.5543387995310098 ) ) ;
#13146 = FACE_OUTER_BOUND ( 'NONE', #11053, .T. ) ;
#13147 = ORIENTED_EDGE ( 'NONE', *, *, #6626, .T. ) ;
#13148 = CARTESIAN_POINT ( 'NONE',  ( 27.03948732994508219, 43.16218137147969003, 78.60433879953099279 ) ) ;
#13149 = CARTESIAN_POINT ( 'NONE',  ( 14.52215374030650175, 44.16218137147969003, 105.5543387995309956 ) ) ;
#13150 = ORIENTED_EDGE ( 'NONE', *, *, #7699, .T. ) ;
#13151 = DIRECTION ( 'NONE',  ( 0.000000000000000000, 0.000000000000000000, 1.000000000000000000 ) ) ;
#13152 = CARTESIAN_POINT ( 'NONE',  ( -4.156427319950602772, 37.43228207296065335, 76.53375056423675460 ) ) ;
#13153 = EDGE_CURVE ( 'NONE', #2164, #5281, #7873, .T. ) ;
#13154 = CARTESIAN_POINT ( 'NONE',  ( -3.981178359372548492, 46.76218137147973408, 96.35183879953099506 ) ) ;
#13155 = ORIENTED_EDGE ( 'NONE', *, *, #13105, .F. ) ;
#13156 = CARTESIAN_POINT ( 'NONE',  ( -4.730130202819499807, 37.10141734037124905, 77.29630340639747033 ) ) ;
#13157 = CARTESIAN_POINT ( 'NONE',  ( -4.483525497724968112, 37.69402149733662810, 77.90854597583356167 ) ) ;
#13158 = CARTESIAN_POINT ( 'NONE',  ( -4.009385194876762704, 46.27527268018315709, 94.51683879953097289 ) ) ;
#13159 = VECTOR ( 'NONE', #10798, 1000.000000000000000 ) ;
#13160 = ORIENTED_EDGE ( 'NONE', *, *, #19238, .T. ) ;
#13161 = CARTESIAN_POINT ( 'NONE',  ( 5.543801380518728728, 50.64470058390610774, 78.66695423199873005 ) ) ;
#13162 = DIRECTION ( 'NONE',  ( 1.540237394707284220E-16, 1.793354297423764243E-16, -1.000000000000000000 ) ) ;
#13163 = CARTESIAN_POINT ( 'NONE',  ( -2.416137431568557314, 39.07291177436112406, 94.86746380123797451 ) ) ;
#13164 = DIRECTION ( 'NONE',  ( 1.000000000000000000, 0.000000000000000000, 0.000000000000000000 ) ) ;
#13165 = CARTESIAN_POINT ( 'NONE',  ( 5.799744778572546444, 50.27941912385354328, 75.41423045364997790 ) ) ;
#13166 = CARTESIAN_POINT ( 'NONE',  ( -4.398409473784897550, 37.60244433931075747, 75.97311671873485750 ) ) ;
#13167 = CARTESIAN_POINT ( 'NONE',  ( 0.3788305629195590774, 52.34483884138099796, 77.02254451525793399 ) ) ;
#13168 = CARTESIAN_POINT ( 'NONE',  ( 5.036257573895150053, 37.49179806381912528, 75.36841521003546518 ) ) ;
#13169 = VECTOR ( 'NONE', #7203, 1000.000000000000227 ) ;
#13170 = ORIENTED_EDGE ( 'NONE', *, *, #16378, .T. ) ;
#13171 = CARTESIAN_POINT ( 'NONE',  ( -5.119673272240743422, 38.21139563191785982, 75.53183897749521236 ) ) ;
#13172 = CARTESIAN_POINT ( 'NONE',  ( 28.52215374030649997, 44.16218137147968292, 87.05433879953099563 ) ) ;
#13173 = DIRECTION ( 'NONE',  ( 5.626130192357176673E-16, 1.809130530872730902E-30, -1.000000000000000000 ) ) ;
#13174 = CARTESIAN_POINT ( 'NONE',  ( 1.136649954779953786, 52.94122945111733003, 79.51059422203249483 ) ) ;
#13175 = VERTEX_POINT ( 'NONE', #740 ) ;
#13176 = ORIENTED_EDGE ( 'NONE', *, *, #6063, .F. ) ;
#13177 = EDGE_CURVE ( 'NONE', #8069, #19924, #1173, .T. ) ;
#13178 = CARTESIAN_POINT ( 'NONE',  ( -3.154801521863568325, 47.83913663364971569, 95.05036078214054385 ) ) ;
#13179 = ORIENTED_EDGE ( 'NONE', *, *, #10429, .F. ) ;
#13180 = AXIS2_PLACEMENT_3D ( 'NONE', #10648, #2749, #7422 ) ;
#13181 = CARTESIAN_POINT ( 'NONE',  ( -4.211488180634966660, 48.16625856408043660, 78.25433879953088478 ) ) ;
#13182 = CARTESIAN_POINT ( 'NONE',  ( 4.531118403667150574, 51.21650232360861565, 77.67439681936272677 ) ) ;
#13183 = DIRECTION ( 'NONE',  ( 1.540237394707284220E-16, 1.793354297423764243E-16, -1.000000000000000000 ) ) ;
#13184 = FACE_OUTER_BOUND ( 'NONE', #19390, .T. ) ;
#13185 = CARTESIAN_POINT ( 'NONE',  ( 2.921181103050038086, 49.30691215337508737, 94.59496379782397923 ) ) ;
#13186 = CARTESIAN_POINT ( 'NONE',  ( -2.416137431568557314, 39.07291177436112406, 93.61746380123804556 ) ) ;
#13187 = AXIS2_PLACEMENT_3D ( 'NONE', #19860, #5282, #15304 ) ;
#13188 = DIRECTION ( 'NONE',  ( -6.067057537060281311E-17, 0.4999999999999999445, -0.8660254037844387076 ) ) ;
#13189 = CARTESIAN_POINT ( 'NONE',  ( -3.053409417734729736, 36.78772418584885884, 76.59109406773794149 ) ) ;
#13190 = FACE_OUTER_BOUND ( 'NONE', #19668, .T. ) ;
#13191 = CARTESIAN_POINT ( 'NONE',  ( 6.198496396448986090, 45.68315280215533392, 92.83621380123798872 ) ) ;
#13192 = ORIENTED_EDGE ( 'NONE', *, *, #14780, .F. ) ;
#13193 = DIRECTION ( 'NONE',  ( -0.5941461771851693774, -0.8043570849667760481, -2.357623395011396791E-16 ) ) ;
#13194 = TOROIDAL_SURFACE ( 'NONE', #5017, 13.99999999999999645, 4.000000000000000000 ) ;
#13195 = ORIENTED_EDGE ( 'NONE', *, *, #3244, .T. ) ;
#13196 = LINE ( 'NONE', #19669, #13304 ) ;
#13197 = CARTESIAN_POINT ( 'NONE',  ( -4.533151836807888913, 37.71055329817392732, 78.64904841171450300 ) ) ;
#13198 = CARTESIAN_POINT ( 'NONE',  ( 8.300051067836092145, 41.58955977690143158, 77.52397343602532942 ) ) ;
#13199 = CARTESIAN_POINT ( 'NONE',  ( 8.435567168294131335, 40.07565444796716747, 75.89798363837520867 ) ) ;
#13200 = ORIENTED_EDGE ( 'NONE', *, *, #13357, .F. ) ;
#13201 = CARTESIAN_POINT ( 'NONE',  ( 6.055654410823096079, 38.22022172098753146, 75.55565825109377442 ) ) ;
#13202 = CARTESIAN_POINT ( 'NONE',  ( 4.577225057937401864, 52.10727814237509392, 78.46169174070733732 ) ) ;
#13203 = CARTESIAN_POINT ( 'NONE',  ( 6.882043956598291601, 37.89095385206773869, 77.31245045813156480 ) ) ;
#13204 = CYLINDRICAL_SURFACE ( 'NONE', #2615, 1.000000000000014655 ) ;
#13205 = CARTESIAN_POINT ( 'NONE',  ( -4.171956714443219916, 37.43867258617596860, 78.78605677924578288 ) ) ;
#13206 = EDGE_LOOP ( 'NONE', ( #14041, #12690, #20323, #9797 ) ) ;
#13207 = APPLICATION_CONTEXT ( 'automotive_design' ) ;
#13208 = CARTESIAN_POINT ( 'NONE',  ( 27.63948732994508006, 36.35905713404685713, 76.90433879953101837 ) ) ;
#13209 = VECTOR ( 'NONE', #2366, 1000.000000000000000 ) ;
#13210 = DIRECTION ( 'NONE',  ( 1.734723475976781654E-15, -1.000000000000000000, 0.000000000000000000 ) ) ;
#13211 = ORIENTED_EDGE ( 'NONE', *, *, #18363, .T. ) ;
#13212 = CARTESIAN_POINT ( 'NONE',  ( -3.350035803220276609, 49.20851703305431357, 91.97683880123797451 ) ) ;
#13213 = EDGE_CURVE ( 'NONE', #10206, #9230, #3010, .T. ) ;
#13214 = CARTESIAN_POINT ( 'NONE',  ( 1.920580872171021358, 52.20313474366393081, 77.08393542551461053 ) ) ;
#13215 = CARTESIAN_POINT ( 'NONE',  ( -3.096372156315136959, 36.80864108843506699, 78.38559710128819802 ) ) ;
#13216 = B_SPLINE_CURVE_WITH_KNOTS ( 'NONE', 3,
 ( #5133, #13237, #5239, #11654, #3649, #8344, #18131, #1759, #8241, #16535, #18022, #10272, #11755, #3551 ),
 .UNSPECIFIED., .F., .F.,
 ( 4, 2, 2, 2, 2, 2, 4 ),
 ( 8.673617379884035472E-19, 0.0002848466061852771079, 0.0004272699092779162311, 0.0005696932123705553000, 0.0007121165154631944232, 0.0008545398185558335464, 0.001139386424741116888 ),
 .UNSPECIFIED. ) ;
#13217 = CARTESIAN_POINT ( 'NONE',  ( 6.012275498921958672, 37.26944915646792822, 78.37198585835440667 ) ) ;
#13218 = VERTEX_POINT ( 'NONE', #2338 ) ;
#13219 = CARTESIAN_POINT ( 'NONE',  ( 10.77494014480653561, 42.96218137147968008, 66.20574467885104752 ) ) ;
#13220 = AXIS2_PLACEMENT_3D ( 'NONE', #1423, #33, #11324 ) ;
#13221 = ADVANCED_FACE ( 'NONE', ( #7442 ), #18928, .T. ) ;
#13222 = ORIENTED_EDGE ( 'NONE', *, *, #1042, .F. ) ;
#13223 = CARTESIAN_POINT ( 'NONE',  ( -7.669666148856070897, 47.37719010417367116, 78.26793921993403558 ) ) ;
#13224 = CARTESIAN_POINT ( 'NONE',  ( 0.5221537403065064087, 48.16218137147969003, 74.55433879953100984 ) ) ;
#13225 = CARTESIAN_POINT ( 'NONE',  ( -0.4699484075730042676, 52.36218137147968577, 48.36106904222365444 ) ) ;
#13226 = VERTEX_POINT ( 'NONE', #7225 ) ;
#13227 = CARTESIAN_POINT ( 'NONE',  ( 8.848467398349676216, 41.31314263134580500, 75.36050707951255845 ) ) ;
#13228 = CARTESIAN_POINT ( 'NONE',  ( 0.5221537403065064087, 48.16218137147969003, 105.5543387995310098 ) ) ;
#13229 = LINE ( 'NONE', #5231, #8128 ) ;
#13230 = CARTESIAN_POINT ( 'NONE',  ( 0.3280703116875920977, 52.35625621862651258, 78.56344688395670062 ) ) ;
#13231 = EDGE_LOOP ( 'NONE', ( #9596, #18238, #15450, #12065, #8168, #10375 ) ) ;
#13232 = CARTESIAN_POINT ( 'NONE',  ( -4.058881954689706362, 50.95759777156840187, 76.06958028623719770 ) ) ;
#13233 = ORIENTED_EDGE ( 'NONE', *, *, #985, .F. ) ;
#13234 = CARTESIAN_POINT ( 'NONE',  ( 2.522153740306511960, 47.62628298661745418, 45.55433879953100273 ) ) ;
#13235 = CARTESIAN_POINT ( 'NONE',  ( -7.428404849043024782, 40.10093606804371547, 78.24455606223649795 ) ) ;
#13236 = VECTOR ( 'NONE', #497, 1000.000000000000000 ) ;
#13237 = CARTESIAN_POINT ( 'NONE',  ( -4.720151432595600660, 37.85605236037169874, 77.33560970407651780 ) ) ;
#13238 = CARTESIAN_POINT ( 'NONE',  ( 0.2860873169776705915, 38.75537135769874197, 93.34496379611698558 ) ) ;
#13239 = EDGE_CURVE ( 'NONE', #5416, #11467, #198, .T. ) ;
#13240 = CARTESIAN_POINT ( 'NONE',  ( 5.453344025566022601, 40.65105419805430387, 75.45433879953087342 ) ) ;
#13241 = CARTESIAN_POINT ( 'NONE',  ( 0.5221537403065006355, 44.16218137147969003, 92.45433879953097289 ) ) ;
#13242 = CARTESIAN_POINT ( 'NONE',  ( -7.086630388250130252, 47.03102748359589214, 77.94747975791852923 ) ) ;
#13243 = AXIS2_PLACEMENT_3D ( 'NONE', #19542, #17848, #20711 ) ;
#13244 = VECTOR ( 'NONE', #18333, 999.9999999999998863 ) ;
#13245 = PRODUCT_RELATED_PRODUCT_CATEGORY ( 'part', '', ( #540 ) ) ;
#13246 = VERTEX_POINT ( 'NONE', #15330 ) ;
#13247 = DIRECTION ( 'NONE',  ( -1.334402673828313339E-16, 1.592765810570777996E-32, 1.000000000000000000 ) ) ;
#13248 = CARTESIAN_POINT ( 'NONE',  ( 5.666494898543479763, 37.02236699927324537, 78.30432351818811298 ) ) ;
#13249 = VERTEX_POINT ( 'NONE', #13723 ) ;
#13250 = DIRECTION ( 'NONE',  ( 0.000000000000000000, 2.168404344970984413E-15, -1.000000000000000000 ) ) ;
#13251 = EDGE_CURVE ( 'NONE', #14909, #19757, #20197, .T. ) ;
#13252 = CARTESIAN_POINT ( 'NONE',  ( 3.502103686363649881, 48.53614194976264429, 92.63161059727374891 ) ) ;
#13253 = CARTESIAN_POINT ( 'NONE',  ( 5.544968037009670780, 45.50804040601273925, 93.38308879953099506 ) ) ;
#13254 = AXIS2_PLACEMENT_3D ( 'NONE', #14438, #3268, #8057 ) ;
#13255 = CARTESIAN_POINT ( 'NONE',  ( -8.264604465707931169, 42.74281979478013938, 76.25640820822667365 ) ) ;
#13256 = ORIENTED_EDGE ( 'NONE', *, *, #8084, .T. ) ;
#13257 = VECTOR ( 'NONE', #20685, 1000.000000000000227 ) ;
#13258 = CARTESIAN_POINT ( 'NONE',  ( -5.281338840898281539, 38.44457945337485683, 75.70067668752250256 ) ) ;
#13260 = ADVANCED_FACE ( 'NONE', ( #14040 ), #20619, .F. ) ;
#13259 = ORIENTED_EDGE ( 'NONE', *, *, #16236, .T. ) ;
#13261 = CARTESIAN_POINT ( 'NONE',  ( 6.489847418355314979, 49.78593742637539776, 78.48669174070734300 ) ) ;
#13262 = CARTESIAN_POINT ( 'NONE',  ( -4.477846259693478714, 37.66295064777091994, 54.55433879953098852 ) ) ;
#13263 = CARTESIAN_POINT ( 'NONE',  ( -2.077846259693550746, 39.65884927180063357, 95.41433879953098085 ) ) ;
#13264 = ORIENTED_EDGE ( 'NONE', *, *, #5198, .T. ) ;
#13265 = DIRECTION ( 'NONE',  ( 1.540237394707284220E-16, 1.793354297423764243E-16, -1.000000000000000000 ) ) ;
#13266 = VECTOR ( 'NONE', #13540, 1000.000000000000000 ) ;
#13267 = ORIENTED_EDGE ( 'NONE', *, *, #15246, .F. ) ;
#13268 = CARTESIAN_POINT ( 'NONE',  ( 0.5221537403065181771, 44.16218137147969003, 56.15433879953099705 ) ) ;
#13269 = CARTESIAN_POINT ( 'NONE',  ( -7.313565574299385474, 41.74526126053015673, 79.54845644658969661 ) ) ;
#13270 = EDGE_CURVE ( 'NONE', #791, #6327, #65, .T. ) ;
#13271 = ADVANCED_FACE ( 'NONE', ( #9369 ), #18208, .T. ) ;
#13272 = EDGE_CURVE ( 'NONE', #11820, #2058, #1862, .T. ) ;
#13273 = EDGE_CURVE ( 'NONE', #347, #7250, #20159, .T. ) ;
#13274 = CARTESIAN_POINT ( 'NONE',  ( 5.620183367589484114, 50.41205390497189143, 75.37891144279687694 ) ) ;
#13275 = CARTESIAN_POINT ( 'NONE',  ( -3.696676068499483048, 37.12873482127974256, 79.45447414167722400 ) ) ;
#13276 = EDGE_CURVE ( 'NONE', #20542, #11018, #8450, .T. ) ;
#13277 = CARTESIAN_POINT ( 'NONE',  ( 4.425132644269478277, 36.13533498154198043, 76.25036098622081226 ) ) ;
#13278 = CARTESIAN_POINT ( 'NONE',  ( 8.386004485381512552, 39.92711194308005673, 78.01856368782078732 ) ) ;
#13279 = ORIENTED_EDGE ( 'NONE', *, *, #8621, .F. ) ;
#13280 = CARTESIAN_POINT ( 'NONE',  ( 0.5221537403065054095, 50.16218137147969713, 83.55433879953099563 ) ) ;
#13281 = CARTESIAN_POINT ( 'NONE',  ( 9.162426004170315608, 42.25409649015283975, 75.50722976489458915 ) ) ;
#13282 = DIRECTION ( 'NONE',  ( 1.540237394707284220E-16, 1.793354297423764243E-16, -1.000000000000000000 ) ) ;
#13283 = DIRECTION ( 'NONE',  ( 1.000000000000000000, 0.000000000000000000, -0.000000000000000000 ) ) ;
#13284 = ORIENTED_EDGE ( 'NONE', *, *, #654, .F. ) ;
#13285 = CARTESIAN_POINT ( 'NONE',  ( 5.791714832554497150, 51.21018346849771063, 78.93490712750880789 ) ) ;
#13286 = ORIENTED_EDGE ( 'NONE', *, *, #4160, .T. ) ;
#13287 = DIRECTION ( 'NONE',  ( 0.000000000000000000, 0.000000000000000000, 1.000000000000000000 ) ) ;
#13288 = CARTESIAN_POINT ( 'NONE',  ( 6.456868491357829143, 49.79402830777683420, 76.00796742194241062 ) ) ;
#13289 = CARTESIAN_POINT ( 'NONE',  ( 9.340212240349364592, 42.78693311852996572, 76.09591779779900378 ) ) ;
#13290 = DIRECTION ( 'NONE',  ( 3.893792155548169402E-16, 7.183611964723547524E-17, -1.000000000000000000 ) ) ;
#13291 = DIRECTION ( 'NONE',  ( -0.9485903129789527988, 0.3165065846431829311, -8.934458285744989980E-17 ) ) ;
#13292 = CARTESIAN_POINT ( 'NONE',  ( 30.92220646078100188, 42.76218137147968434, 62.80715055817104542 ) ) ;
#13293 = LINE ( 'NONE', #19865, #5212 ) ;
#13294 = B_SPLINE_SURFACE_WITH_KNOTS ( 'NONE', 3, 1, ( 
 ( #16448, #10064 ),
 ( #18139, #1768 ),
 ( #11762, #14939 ),
 ( #11864, #13139 ),
 ( #16546, #1867 ),
 ( #13248, #8458 ),
 ( #18237, #16649 ),
 ( #2071, #467 ),
 ( #14705, #17507 ),
 ( #9434, #11421 ),
 ( #13217, #13428 ) ),
 .UNSPECIFIED., .F., .F., .F.,
 ( 4, 1, 1, 1, 1, 1, 1, 1, 4 ),
 ( 2, 2 ),
 ( 0.000000000000000000, 0.1208544691022559597, 0.2402546218586821825, 0.3598696579477268509, 0.4809300011950208842, 0.6037041574249993880, 0.7308714335393303729, 0.8631644367168944676, 0.9999999999999998890 ),
 ( 0.000000000000000000, 1.000000000000000000 ),
 .UNSPECIFIED. ) ;
#13295 = DIRECTION ( 'NONE',  ( -9.598494438985367424E-18, 5.922860397471809309E-17, -1.000000000000000000 ) ) ;
#13296 = PLANE ( 'NONE',  #5766 ) ;
#13297 = CARTESIAN_POINT ( 'NONE',  ( 4.694131320935415630, 52.02092419516998234, 75.77039595153209461 ) ) ;
#13298 = EDGE_CURVE ( 'NONE', #682, #14937, #19591, .T. ) ;
#13299 = CARTESIAN_POINT ( 'NONE',  ( 1.352400422481993658, 50.46853102219002096, 90.57058880123798872 ) ) ;
#13300 = CARTESIAN_POINT ( 'NONE',  ( -4.524181921268124462, 40.28999182795290324, 91.03933880123798872 ) ) ;
#13301 = ORIENTED_EDGE ( 'NONE', *, *, #6580, .T. ) ;
#13302 = ADVANCED_FACE ( 'NONE', ( #11970 ), #13448, .T. ) ;
#13303 = CARTESIAN_POINT ( 'NONE',  ( 4.080804472568812180, 36.77439181754974840, 75.94166117767865387 ) ) ;
#13304 = VECTOR ( 'NONE', #19776, 999.9999999999998863 ) ;
#13305 = CARTESIAN_POINT ( 'NONE',  ( 31.22215374030650281, 42.76218137147968434, 78.80433879953099563 ) ) ;
#13306 = CARTESIAN_POINT ( 'NONE',  ( -4.525718010196823293, 37.70506222990913869, 78.74088963820604192 ) ) ;
#13307 = VECTOR ( 'NONE', #8795, 1000.000000000000000 ) ;
#13308 = DIRECTION ( 'NONE',  ( -1.540237394707284220E-16, -1.793354297423764243E-16, 1.000000000000000000 ) ) ;
#13309 = FACE_OUTER_BOUND ( 'NONE', #3846, .T. ) ;
#13310 = EDGE_CURVE ( 'NONE', #20868, #6298, #8348, .T. ) ;
#13311 = CARTESIAN_POINT ( 'NONE',  ( 9.353817388681445522, 42.82770861117572281, 78.41904468188381827 ) ) ;
#13312 = ORIENTED_EDGE ( 'NONE', *, *, #4327, .F. ) ;
#13313 = AXIS2_PLACEMENT_3D ( 'NONE', #7657, #14239, #2869 ) ;
#13314 = CARTESIAN_POINT ( 'NONE',  ( 5.868769507328080337, 38.08668061124301829, 78.34126521887253602 ) ) ;
#13315 = DIRECTION ( 'NONE',  ( 0.3165065846431827645, 0.9485903129789529098, 0.000000000000000000 ) ) ;
#13316 = CARTESIAN_POINT ( 'NONE',  ( 0.8456863967494556711, 52.95623207773213181, 76.19861728079081331 ) ) ;
#13317 = ORIENTED_EDGE ( 'NONE', *, *, #17821, .F. ) ;
#13318 = VECTOR ( 'NONE', #5071, 1000.000000000000114 ) ;
#13319 = LINE ( 'NONE', #8101, #19942 ) ;
#13320 = LINE ( 'NONE', #7016, #7148 ) ;
#13321 = ORIENTED_EDGE ( 'NONE', *, *, #20016, .F. ) ;
#13322 = CARTESIAN_POINT ( 'NONE',  ( 5.611423337425062385, 41.22389019960463230, 90.17996380123798872 ) ) ;
#13323 = CARTESIAN_POINT ( 'NONE',  ( 2.114319545972857650, 52.20160704302087140, 77.78911287202200242 ) ) ;
#13324 = CARTESIAN_POINT ( 'NONE',  ( -4.524181921268124462, 40.28999182795290324, 91.19558880123797451 ) ) ;
#13325 = AXIS2_PLACEMENT_3D ( 'NONE', #18368, #593, #5267 ) ;
#13326 = CARTESIAN_POINT ( 'NONE',  ( 8.332139447377956643, 41.66172086508280614, 79.54742650360671519 ) ) ;
#13327 = VERTEX_POINT ( 'NONE', #8672 ) ;
#13328 = AXIS2_PLACEMENT_3D ( 'NONE', #4890, #8099, #12997 ) ;
#13329 = LINE ( 'NONE', #5008, #10306 ) ;
#13330 = VERTEX_POINT ( 'NONE', #14830 ) ;
#13331 = DIRECTION ( 'NONE',  ( -0.9485903129789529098, 0.3165065846431826535, -8.934458285744997376E-17 ) ) ;
#13332 = CARTESIAN_POINT ( 'NONE',  ( 1.352400422481993658, 50.46853102219002096, 95.57058880123798872 ) ) ;
#13333 = EDGE_LOOP ( 'NONE', ( #3623, #8176, #16190, #7115 ) ) ;
#13334 = CARTESIAN_POINT ( 'NONE',  ( 2.421193248165596668, 49.85372324935340060, 80.45433879953087342 ) ) ;
#13335 = CARTESIAN_POINT ( 'NONE',  ( 8.133552201135486825, 41.55168119144260430, 75.36050707951255845 ) ) ;
#13336 = CARTESIAN_POINT ( 'NONE',  ( 6.020541483214493894, 43.49297395252375509, 92.55433879953095300 ) ) ;
#13337 = CARTESIAN_POINT ( 'NONE',  ( -4.398802922602397913, 51.46161812541917868, 78.75145056212190298 ) ) ;
#13338 = CARTESIAN_POINT ( 'NONE',  ( 0.3769493647919933688, 52.96722407749858519, 78.82913797267801215 ) ) ;
#13339 = ORIENTED_EDGE ( 'NONE', *, *, #8590, .T. ) ;
#13340 = CARTESIAN_POINT ( 'NONE',  ( -4.239546901740170348, 50.82850121497202167, 75.97198585835440099 ) ) ;
#13341 = CIRCLE ( 'NONE', #1473, 4.000000000000003553 ) ;
#13342 = VERTEX_POINT ( 'NONE', #15153 ) ;
#13343 = CARTESIAN_POINT ( 'NONE',  ( 0.5221537403065015237, 44.16218137147968292, 75.45433879953087342 ) ) ;
#13344 = CARTESIAN_POINT ( 'NONE',  ( 2.122153740306511160, 47.82824192744436687, 61.55433879953100273 ) ) ;
#13345 = AXIS2_PLACEMENT_3D ( 'NONE', #19452, #4868, #16797 ) ;
#13346 = DIRECTION ( 'NONE',  ( -0.9485903129789527988, 0.3165065846431829311, -8.934458285744989980E-17 ) ) ;
#13347 = CARTESIAN_POINT ( 'NONE',  ( -4.884656273474451638, 44.39824779480852612, 94.28246379611698558 ) ) ;
#13348 = CARTESIAN_POINT ( 'NONE',  ( -1.876873622437039257, 39.01745058958429269, 92.87621379782399345 ) ) ;
#13349 = CARTESIAN_POINT ( 'NONE',  ( 5.488638308869484561, 37.64219262425781665, 76.17246542145134924 ) ) ;
#13350 = CARTESIAN_POINT ( 'NONE',  ( -4.089052737068717747, 51.68295426732343856, 75.42336258079946276 ) ) ;
#13351 = VERTEX_POINT ( 'NONE', #14729 ) ;
#13352 = DIRECTION ( 'NONE',  ( 1.540237394707284220E-16, 1.793354297423764243E-16, -1.000000000000000000 ) ) ;
#13353 = CARTESIAN_POINT ( 'NONE',  ( 2.722153740306501479, 44.16218137147969003, 37.95170767603170248 ) ) ;
#13354 = ORIENTED_EDGE ( 'NONE', *, *, #14148, .F. ) ;
#13355 = AXIS2_PLACEMENT_3D ( 'NONE', #11720, #16602, #18292 ) ;
#13356 = CARTESIAN_POINT ( 'NONE',  ( -7.677846259693481556, 40.96218137147969429, 80.55433879953099563 ) ) ;
#13357 = EDGE_CURVE ( 'NONE', #4192, #158, #150, .T. ) ;
#13358 = DIRECTION ( 'NONE',  ( 1.540237394707284220E-16, 1.793354297423764243E-16, -1.000000000000000000 ) ) ;
#13359 = CARTESIAN_POINT ( 'NONE',  ( 6.102441102155617969, 43.42752260303680600, 92.05496379953099506 ) ) ;
#13360 = ORIENTED_EDGE ( 'NONE', *, *, #7398, .F. ) ;
#13361 = CARTESIAN_POINT ( 'NONE',  ( 8.879174460483845621, 41.40517364458161609, 78.05744560429982926 ) ) ;
#13362 = CARTESIAN_POINT ( 'NONE',  ( -4.716387082485078430, 37.09126585098686490, 75.36022115247205022 ) ) ;
#13363 = ORIENTED_EDGE ( 'NONE', *, *, #16254, .F. ) ;
#13364 = DIRECTION ( 'NONE',  ( -0.7071067811865434649, 0.7071067811865515695, 0.000000000000000000 ) ) ;
#13365 = CARTESIAN_POINT ( 'NONE',  ( 0.3326973149608341562, 52.96014171822455552, 76.44919174070734869 ) ) ;
#13366 = ORIENTED_EDGE ( 'NONE', *, *, #18579, .T. ) ;
#13367 = DIRECTION ( 'NONE',  ( -0.8043570849667761591, 0.5941461771851692664, -1.733862608106489734E-17 ) ) ;
#13368 = CARTESIAN_POINT ( 'NONE',  ( 5.611423337425062385, 41.22389019960463230, 94.08621380123797451 ) ) ;
#13369 = VERTEX_POINT ( 'NONE', #19719 ) ;
#13370 = CARTESIAN_POINT ( 'NONE',  ( 2.350558581813037673, 49.87752504164859602, 61.32593395802448555 ) ) ;
#13371 = DIRECTION ( 'NONE',  ( -1.000000000000000000, -1.402518428993831676E-16, 7.152522014899655971E-33 ) ) ;
#13372 = VECTOR ( 'NONE', #3739, 1000.000000000000000 ) ;
#13373 =( LENGTH_UNIT ( ) NAMED_UNIT ( * ) SI_UNIT ( .MILLI., .METRE. ) );
#13374 = EDGE_CURVE ( 'NONE', #7434, #19503, #19608, .T. ) ;
#13375 = CARTESIAN_POINT ( 'NONE',  ( 4.178421596892070156, 40.17206517740157778, 93.81371379953098710 ) ) ;
#13376 = FACE_OUTER_BOUND ( 'NONE', #8499, .T. ) ;
#13377 = EDGE_LOOP ( 'NONE', ( #13420, #10293, #13692, #20267 ) ) ;
#13378 = ORIENTED_EDGE ( 'NONE', *, *, #14969, .F. ) ;
#13379 = CARTESIAN_POINT ( 'NONE',  ( 5.116981105040771638, 36.62970456142029008, 75.43572969368668168 ) ) ;
#13380 = EDGE_CURVE ( 'NONE', #12382, #13012, #18655, .T. ) ;
#13381 = CARTESIAN_POINT ( 'NONE',  ( 7.682243507100542601, 40.18231369592098190, 78.58253683706189463 ) ) ;
#13382 = ORIENTED_EDGE ( 'NONE', *, *, #12249, .T. ) ;
#13383 = DIRECTION ( 'NONE',  ( -0.3165065846431827090, -0.9485903129789527988, 0.000000000000000000 ) ) ;
#13384 = DIRECTION ( 'NONE',  ( 3.211742425186504723E-16, -5.922860397471811774E-17, 1.000000000000000000 ) ) ;
#13385 = CARTESIAN_POINT ( 'NONE',  ( 2.043125170982144745, 38.48583871533720213, 93.92996380123798872 ) ) ;
#13386 = EDGE_CURVE ( 'NONE', #4079, #16470, #17376, .T. ) ;
#13387 = VERTEX_POINT ( 'NONE', #8989 ) ;
#13388 = ORIENTED_EDGE ( 'NONE', *, *, #13676, .F. ) ;
#13389 = AXIS2_PLACEMENT_3D ( 'NONE', #4769, #15862, #1278 ) ;
#13390 = DIRECTION ( 'NONE',  ( 0.007885122365275663500, 0.9999689119394085113, 1.805443505845543142E-16 ) ) ;
#13391 = EDGE_LOOP ( 'NONE', ( #15147, #6777, #19533, #11451 ) ) ;
#13392 = CARTESIAN_POINT ( 'NONE',  ( -2.083470957239373256, 47.45622447009557021, 82.45433879953087342 ) ) ;
#13393 = DIRECTION ( 'NONE',  ( -3.211742425186504723E-16, 5.922860397471811774E-17, -1.000000000000000000 ) ) ;
#13394 = CARTESIAN_POINT ( 'NONE',  ( -2.919077339881743782, 51.60516013878824992, 78.30927351043679607 ) ) ;
#13395 = ADVANCED_FACE ( 'NONE', ( #4278 ), #16955, .F. ) ;
#13396 = CARTESIAN_POINT ( 'NONE',  ( -0.9228510475973594751, 52.84273317725999419, 76.37557405286315770 ) ) ;
#13397 = CARTESIAN_POINT ( 'NONE',  ( -4.007890887056452023, 40.01116025973682611, 93.89183879782397923 ) ) ;
#13398 = CARTESIAN_POINT ( 'NONE',  ( 0.8503868799515119647, 52.96349134317159013, 77.76169174070734869 ) ) ;
#13399 = FACE_OUTER_BOUND ( 'NONE', #18951, .T. ) ;
#13400 = PLANE ( 'NONE',  #19374 ) ;
#13401 = CARTESIAN_POINT ( 'NONE',  ( 4.454347278305088587, 39.79502279609036464, 90.11785590924256439 ) ) ;
#13402 = VERTEX_POINT ( 'NONE', #8772 ) ;
#13403 = CARTESIAN_POINT ( 'NONE',  ( 4.252632704766235783, 36.85940042850018017, 75.70221307569202907 ) ) ;
#13404 = ORIENTED_EDGE ( 'NONE', *, *, #1901, .F. ) ;
#13405 = CARTESIAN_POINT ( 'NONE',  ( -3.226449543290886179, 47.76606447477297479, 92.55433879953076826 ) ) ;
#13406 = CARTESIAN_POINT ( 'NONE',  ( 2.722153740306518799, 47.73989013547934945, 54.55433879953099563 ) ) ;
#13407 = CARTESIAN_POINT ( 'NONE',  ( 0.3821786226492928651, 35.36301154328572949, 75.45433879953087342 ) ) ;
#13408 = CARTESIAN_POINT ( 'NONE',  ( -0.9988176903691428077, 49.83852402762217082, 93.30496380123798872 ) ) ;
#13409 = EDGE_CURVE ( 'NONE', #8044, #8009, #6552, .T. ) ;
#13410 = LINE ( 'NONE', #3609, #13946 ) ;
#13411 = DIRECTION ( 'NONE',  ( 1.290716872006552287E-16, 1.000000000000000000, 0.000000000000000000 ) ) ;
#13412 = ADVANCED_BREP_SHAPE_REPRESENTATION ( '', ( #18516, #18366 ), #19057 ) ;
#13413 = EDGE_CURVE ( 'NONE', #4650, #10809, #4074, .T. ) ;
#13414 = CARTESIAN_POINT ( 'NONE',  ( 5.202885763635528349, 50.89499265101085967, 76.39036821129558064 ) ) ;
#13415 = VERTEX_POINT ( 'NONE', #18552 ) ;
#13416 = CARTESIAN_POINT ( 'NONE',  ( 8.625916568955123154, 43.01056172780193521, 78.83313045764568017 ) ) ;
#13417 = PLANE ( 'NONE',  #17897 ) ;
#13418 = EDGE_CURVE ( 'NONE', #3669, #16858, #20235, .T. ) ;
#13419 = PLANE ( 'NONE',  #15389 ) ;
#13420 = ORIENTED_EDGE ( 'NONE', *, *, #19345, .T. ) ;
#13421 = CARTESIAN_POINT ( 'NONE',  ( -4.812918938429301186, 42.57296343998554988, 95.05433879953095300 ) ) ;
#13422 = EDGE_CURVE ( 'NONE', #13387, #8823, #1742, .T. ) ;
#13423 = CARTESIAN_POINT ( 'NONE',  ( 9.539487329945091076, 44.16218137147969713, 75.00433879953099847 ) ) ;
#13424 = CARTESIAN_POINT ( 'NONE',  ( 1.256812508749381774, 49.74246873332880625, 93.92996380294498238 ) ) ;
#13425 = ADVANCED_FACE ( 'NONE', ( #7794 ), #15796, .F. ) ;
#13426 = CARTESIAN_POINT ( 'NONE',  ( 2.120831115265152444, 52.94022022329007626, 77.84551527011910821 ) ) ;
#13427 = CARTESIAN_POINT ( 'NONE',  ( 6.828503391016846891, 43.33193468930419101, 90.41433880123798872 ) ) ;
#13428 = CARTESIAN_POINT ( 'NONE',  ( 5.653812050471574757, 37.77110297002621309, 78.37198585835440667 ) ) ;
#13429 = ORIENTED_EDGE ( 'NONE', *, *, #13589, .F. ) ;
#13430 = DIRECTION ( 'NONE',  ( 1.000000000000000000, -0.000000000000000000, -0.000000000000000000 ) ) ;
#13431 = EDGE_LOOP ( 'NONE', ( #10822, #1916, #17641, #4199 ) ) ;
#13432 = CARTESIAN_POINT ( 'NONE',  ( -4.895593109503407092, 37.22363812428621088, 77.05433879953086773 ) ) ;
#13433 = CARTESIAN_POINT ( 'NONE',  ( 4.394343283833276992, 39.11584570990505938, 92.60183880123797451 ) ) ;
#13434 = VERTEX_POINT ( 'NONE', #14172 ) ;
#13435 = CARTESIAN_POINT ( 'NONE',  ( 8.344059103522193155, 41.69997857441280331, 78.09649493259128405 ) ) ;
#13436 = CARTESIAN_POINT ( 'NONE',  ( 2.263811127080454622, 49.90383875825364157, 69.41268141275703840 ) ) ;
#13437 = DIRECTION ( 'NONE',  ( -1.540237394707283727E-16, -1.793354297423763257E-16, 1.000000000000000000 ) ) ;
#13438 = EDGE_CURVE ( 'NONE', #14937, #18369, #1279, .T. ) ;
#13439 = CARTESIAN_POINT ( 'NONE',  ( -1.187946976321871961, 48.86064447540922373, 93.11058879953097289 ) ) ;
#13440 = EDGE_LOOP ( 'NONE', ( #16340, #2839, #2819, #1360 ) ) ;
#13441 = DIRECTION ( 'NONE',  ( -0.3181025035074024898, 0.9480563259966799938, 1.210247515173824561E-16 ) ) ;
#13442 = ORIENTED_EDGE ( 'NONE', *, *, #20934, .T. ) ;
#13443 = DIRECTION ( 'NONE',  ( -1.540237394707284220E-16, -1.793354297423764243E-16, 1.000000000000000000 ) ) ;
#13444 = CARTESIAN_POINT ( 'NONE',  ( -6.882752284265650111, 40.85947821762912469, 77.28168744664917256 ) ) ;
#13445 = CARTESIAN_POINT ( 'NONE',  ( 5.508100443945853186, 47.59510827513957310, 72.45432679953087529 ) ) ;
#13446 = CARTESIAN_POINT ( 'NONE',  ( -7.782479702508445563, 41.24717501159041433, 76.51864607170344357 ) ) ;
#13447 = CARTESIAN_POINT ( 'NONE',  ( -4.007890887056452023, 40.01116025973682611, 94.04808879782397923 ) ) ;
#13448 = CYLINDRICAL_SURFACE ( 'NONE', #3463, 4.999999999999997335 ) ;
#13449 = ORIENTED_EDGE ( 'NONE', *, *, #16378, .F. ) ;
#13450 = CARTESIAN_POINT ( 'NONE',  ( 0.5221537403065010796, 44.16218137147968292, 78.41904468188380406 ) ) ;
#13451 = DIRECTION ( 'NONE',  ( -1.540237394707284220E-16, -1.793354297423764243E-16, 1.000000000000000000 ) ) ;
#13452 = EDGE_LOOP ( 'NONE', ( #18214, #4894, #12521, #17105 ) ) ;
#13453 = LINE ( 'NONE', #5353, #17660 ) ;
#13454 = CARTESIAN_POINT ( 'NONE',  ( -5.058133621542618030, 44.89684013992257405, 93.92996379953099506 ) ) ;
#13455 = CARTESIAN_POINT ( 'NONE',  ( 1.256812508749381774, 49.74246873332880625, 96.11746379953099506 ) ) ;
#13456 = PRODUCT_DEFINITION_SHAPE ( 'NONE', 'NONE',  #17682 ) ;
#13457 = EDGE_LOOP ( 'NONE', ( #13842, #14642, #16130, #4539 ) ) ;
#13458 = DIRECTION ( 'NONE',  ( -1.196361017915039239E-16, 0.000000000000000000, 1.000000000000000000 ) ) ;
#13459 = CARTESIAN_POINT ( 'NONE',  ( -5.868264228364995283, 37.94211109820661676, 75.91870325888974946 ) ) ;
#13460 = ORIENTED_EDGE ( 'NONE', *, *, #7164, .F. ) ;
#13461 = CARTESIAN_POINT ( 'NONE',  ( -1.376885767552596063, 38.47063949360596524, 82.45433879953087342 ) ) ;
#13462 = CARTESIAN_POINT ( 'NONE',  ( 0.4199111084294616658, 52.96161903445963759, 76.98462281259935480 ) ) ;
#13463 = ORIENTED_EDGE ( 'NONE', *, *, #6872, .T. ) ;
#13464 = CARTESIAN_POINT ( 'NONE',  ( -4.208505828092586221, 37.49087554584724558, 78.00876120161012750 ) ) ;
#13465 = CARTESIAN_POINT ( 'NONE',  ( -0.9988176903691428077, 49.83852402762217082, 94.55496380123798872 ) ) ;
#13466 = ORIENTED_EDGE ( 'NONE', *, *, #7667, .F. ) ;
#13467 = CARTESIAN_POINT ( 'NONE',  ( -4.649709362898930998, 51.28232956945436882, 75.97399450257033493 ) ) ;
#13468 = LINE ( 'NONE', #379, #2727 ) ;
#13469 = VECTOR ( 'NONE', #13393, 1000.000000000000000 ) ;
#13470 = CARTESIAN_POINT ( 'NONE',  ( 8.207311740369052089, 47.02196222218739763, 75.43669174070734584 ) ) ;
#13471 = EDGE_CURVE ( 'NONE', #9413, #9222, #2804, .T. ) ;
#13472 = LINE ( 'NONE', #10194, #1106 ) ;
#13473 = ORIENTED_EDGE ( 'NONE', *, *, #16686, .F. ) ;
#13474 = CYLINDRICAL_SURFACE ( 'NONE', #16975, 6.000000000000002665 ) ;
#13475 = VERTEX_POINT ( 'NONE', #11318 ) ;
#13476 = LINE ( 'NONE', #394, #16290 ) ;
#13477 = CARTESIAN_POINT ( 'NONE',  ( 25.03948732994508219, 36.35905713404684292, 74.70433879953100131 ) ) ;
#13478 = CARTESIAN_POINT ( 'NONE',  ( 3.460444912181559474, 49.25145096859824889, 95.64871380123798872 ) ) ;
#13479 = ORIENTED_EDGE ( 'NONE', *, *, #1932, .F. ) ;
#13480 = EDGE_CURVE ( 'NONE', #9281, #8992, #12695, .T. ) ;
#13481 = VECTOR ( 'NONE', #18197, 1000.000000000000000 ) ;
#13482 = CARTESIAN_POINT ( 'NONE',  ( 27.03948732994508219, 27.61837231449496599, 75.00433879953101268 ) ) ;
#13483 = VERTEX_POINT ( 'NONE', #17791 ) ;
#13484 = CARTESIAN_POINT ( 'NONE',  ( -3.955205046931956403, 36.52901134360649138, 77.68963291717793140 ) ) ;
#13485 = CARTESIAN_POINT ( 'NONE',  ( 8.621533274486752774, 40.63300666569625008, 75.47105533938442079 ) ) ;
#13486 = B_SPLINE_CURVE_WITH_KNOTS ( 'NONE', 3,
 ( #17631, #14652, #16258, #80 ),
 .UNSPECIFIED., .F., .F.,
 ( 4, 4 ),
 ( 0.01304472255648662232, 0.01428392225856177540 ),
 .UNSPECIFIED. ) ;
#13487 = CARTESIAN_POINT ( 'NONE',  ( 6.198496396448986090, 45.68315280215533392, 92.83621380123807398 ) ) ;
#13488 = CARTESIAN_POINT ( 'NONE',  ( -4.225462782839600528, 50.84799750334796187, 79.54845644658969661 ) ) ;
#13489 = CARTESIAN_POINT ( 'NONE',  ( 0.3575591894758495259, 52.96144190202271318, 75.36602842597199015 ) ) ;
#13490 = CARTESIAN_POINT ( 'NONE',  ( -4.524181921268124462, 40.28999182795290324, 96.19558880123798872 ) ) ;
#13491 = CARTESIAN_POINT ( 'NONE',  ( 8.292349522058055200, 41.56647775562769453, 75.97198585835440099 ) ) ;
#13492 = CARTESIAN_POINT ( 'NONE',  ( -7.677846259693484221, 40.96218137147969429, 53.35433879953099989 ) ) ;
#13493 = LINE ( 'NONE', #11605, #5098 ) ;
#13494 = CARTESIAN_POINT ( 'NONE',  ( 6.828503391016846891, 43.33193468930419101, 90.25808880123800293 ) ) ;
#13495 = VECTOR ( 'NONE', #21010, 1000.000000000000114 ) ;
#13496 = FACE_OUTER_BOUND ( 'NONE', #16657, .T. ) ;
#13497 = ORIENTED_EDGE ( 'NONE', *, *, #8342, .F. ) ;
#13498 = CARTESIAN_POINT ( 'NONE',  ( 0.3616762838632459620, 52.96733004806014122, 76.07436980028356288 ) ) ;
#13499 = DIRECTION ( 'NONE',  ( -1.402518428993831676E-16, 1.000000000000000000, -0.000000000000000000 ) ) ;
#13500 = DIRECTION ( 'NONE',  ( 3.893792155548169402E-16, 7.183611964723547524E-17, -1.000000000000000000 ) ) ;
#13501 = CARTESIAN_POINT ( 'NONE',  ( -4.889784912074390810, 37.21934784281386044, 78.69750623079058016 ) ) ;
#13502 = CARTESIAN_POINT ( 'NONE',  ( 4.001624342216747010, 40.29782057951908314, 90.66473080991372058 ) ) ;
#13503 = AXIS2_PLACEMENT_3D ( 'NONE', #13104, #14484, #8210 ) ;
#13504 = DIRECTION ( 'NONE',  ( 0.000000000000000000, -0.000000000000000000, 1.000000000000000000 ) ) ;
#13505 = ADVANCED_FACE ( 'NONE', ( #23 ), #20959, .T. ) ;
#13506 = CARTESIAN_POINT ( 'NONE',  ( 5.459965721645525960, 50.70211769645560906, 77.96367690144739981 ) ) ;
#13507 = ORIENTED_EDGE ( 'NONE', *, *, #10138, .F. ) ;
#13508 = VECTOR ( 'NONE', #825, 1000.000000000000000 ) ;
#13509 = CARTESIAN_POINT ( 'NONE',  ( 8.953205446347402230, 41.62704920565285249, 79.54154676390322720 ) ) ;
#13510 = LINE ( 'NONE', #19987, #7733 ) ;
#13511 = DIRECTION ( 'NONE',  ( 1.540237394707284220E-16, 1.793354297423764243E-16, -1.000000000000000000 ) ) ;
#13512 = ORIENTED_EDGE ( 'NONE', *, *, #20609, .T. ) ;
#13513 = CARTESIAN_POINT ( 'NONE',  ( 0.5221537403065020788, 52.36218137147968577, 48.36106904222365444 ) ) ;
#13514 = CARTESIAN_POINT ( 'NONE',  ( -4.756326795192973300, 45.27753124462999779, 95.05433879953100984 ) ) ;
#13515 = DIRECTION ( 'NONE',  ( -1.110223024625156540E-16, -1.000000000000000000, -5.922860397471808077E-17 ) ) ;
#13516 = CARTESIAN_POINT ( 'NONE',  ( -2.904223097202481174, 48.62752260303690122, 90.33621380294496817 ) ) ;
#13517 = EDGE_CURVE ( 'NONE', #13475, #14379, #17482, .T. ) ;
#13518 = VECTOR ( 'NONE', #11183, 1000.000000000000000 ) ;
#13519 = CARTESIAN_POINT ( 'NONE',  ( 2.050865772649529628, 52.20210739934316990, 77.29915700192239569 ) ) ;
#13520 = ADVANCED_FACE ( 'NONE', ( #14278 ), #7695, .F. ) ;
#13521 = CARTESIAN_POINT ( 'NONE',  ( 4.394343283833276992, 39.11584570990505938, 95.10183880123797451 ) ) ;
#13522 = LINE ( 'NONE', #15553, #20750 ) ;
#13523 = ORIENTED_EDGE ( 'NONE', *, *, #17193, .F. ) ;
#13524 = ADVANCED_FACE ( 'NONE', ( #15890 ), #11418, .F. ) ;
#13525 = CARTESIAN_POINT ( 'NONE',  ( -4.477846259693498254, 37.66218137147969713, 53.35433879953099989 ) ) ;
#13526 = EDGE_CURVE ( 'NONE', #20602, #14974, #19173, .T. ) ;
#13527 = ORIENTED_EDGE ( 'NONE', *, *, #14201, .F. ) ;
#13528 = DIRECTION ( 'NONE',  ( -0.3165065846431826535, -0.9485903129789529098, -2.188653791613874008E-16 ) ) ;
#13529 = CARTESIAN_POINT ( 'NONE',  ( -0.3080929418689875576, 37.85583172076933778, 91.19558880123798872 ) ) ;
#13530 = ADVANCED_FACE ( 'NONE', ( #11210 ), #18560, .F. ) ;
#13531 = ORIENTED_EDGE ( 'NONE', *, *, #6800, .F. ) ;
#13532 = DIRECTION ( 'NONE',  ( 1.779391786395883536E-16, 5.922860397471806844E-17, -1.000000000000000000 ) ) ;
#13533 = VECTOR ( 'NONE', #19078, 1000.000000000000000 ) ;
#13534 = CARTESIAN_POINT ( 'NONE',  ( -3.944959226007137776, 38.51060946023304865, 78.53742703482498655 ) ) ;
#13535 = CARTESIAN_POINT ( 'NONE',  ( -3.448881463449838591, 52.14039722128521959, 78.93778436892569061 ) ) ;
#13536 = DIRECTION ( 'NONE',  ( -1.000000000000000000, 1.110223024625156540E-16, -1.779391786395883043E-16 ) ) ;
#13537 = CARTESIAN_POINT ( 'NONE',  ( 5.244536171700299398, 50.85972636156689219, 77.21343514867072599 ) ) ;
#13538 = CARTESIAN_POINT ( 'NONE',  ( 0.3361279572737660426, 52.96754596929898184, 78.62228161321135644 ) ) ;
#13539 = ORIENTED_EDGE ( 'NONE', *, *, #12879, .F. ) ;
#13540 = DIRECTION ( 'NONE',  ( 3.893792155548169402E-16, 7.183611964723547524E-17, -1.000000000000000000 ) ) ;
#13541 = EDGE_LOOP ( 'NONE', ( #3831, #18111, #16792, #12622 ) ) ;
#13542 = LINE ( 'NONE', #16849, #15877 ) ;
#13543 = CARTESIAN_POINT ( 'NONE',  ( 6.737194059699555204, 50.51179604963209613, 77.55733179791843668 ) ) ;
#13544 = LINE ( 'NONE', #20232, #18811 ) ;
#13545 = PLANE ( 'NONE',  #1651 ) ;
#13546 = CARTESIAN_POINT ( 'NONE',  ( 5.052198367669452850, 48.31320248322254685, 94.51683879782399345 ) ) ;
#13547 = CARTESIAN_POINT ( 'NONE',  ( 5.845446004764687231, 37.15023890796076245, 76.33129752952908120 ) ) ;
#13548 = VECTOR ( 'NONE', #20946, 1000.000000000000000 ) ;
#13549 = ORIENTED_EDGE ( 'NONE', *, *, #16424, .T. ) ;
#13550 = EDGE_CURVE ( 'NONE', #4385, #15280, #20080, .T. ) ;
#13551 = CARTESIAN_POINT ( 'NONE',  ( 8.260815876642354283, 41.47217187522794291, 78.92656146296575059 ) ) ;
#13552 = EDGE_LOOP ( 'NONE', ( #2573, #6320, #1686, #7147 ) ) ;
#13553 = DIRECTION ( 'NONE',  ( -0.007885122365285377952, -0.9999689119394085113, -1.805443505845558427E-16 ) ) ;
#13554 = CARTESIAN_POINT ( 'NONE',  ( 1.868012774839550749, 39.13936707477651566, 94.32058879953099506 ) ) ;
#13555 = CARTESIAN_POINT ( 'NONE',  ( -2.904223097202481174, 48.62752260303690122, 95.02371379953099506 ) ) ;
#13556 = ORIENTED_EDGE ( 'NONE', *, *, #4933, .T. ) ;
#13557 = CARTESIAN_POINT ( 'NONE',  ( 10.77494014480653561, 42.76218137147968434, 65.80574467885102763 ) ) ;
#13558 = CARTESIAN_POINT ( 'NONE',  ( -3.416655825507938449, 49.09312776965069958, 94.48111517502780998 ) ) ;
#13559 = ORIENTED_EDGE ( 'NONE', *, *, #2981, .F. ) ;
#13560 = LINE ( 'NONE', #5470, #12857 ) ;
#13561 = CARTESIAN_POINT ( 'NONE',  ( -4.804325902087982492, 51.17184625142267151, 78.52518475144754007 ) ) ;
#13562 = EDGE_LOOP ( 'NONE', ( #13429, #15823, #9242, #20380 ) ) ;
#13563 = LINE ( 'NONE', #18463, #7123 ) ;
#13564 = VECTOR ( 'NONE', #10146, 1000.000000000000000 ) ;
#13565 = CARTESIAN_POINT ( 'NONE',  ( 4.987494971863720927, 47.58855820898865829, 90.96121379953099506 ) ) ;
#13566 = ORIENTED_EDGE ( 'NONE', *, *, #1286, .T. ) ;
#13567 = CARTESIAN_POINT ( 'NONE',  ( 0.6306725468420852909, 52.36149037339925627, 77.38615272760776520 ) ) ;
#13568 = PLANE ( 'NONE',  #17659 ) ;
#13569 = VECTOR ( 'NONE', #17434, 1000.000000000000000 ) ;
#13570 = SHAPE_DEFINITION_REPRESENTATION ( #13456, #14198 ) ;
#13571 = CARTESIAN_POINT ( 'NONE',  ( -4.842431058766297980, 37.18436945890473311, 76.00936707281648808 ) ) ;
#13572 = CARTESIAN_POINT ( 'NONE',  ( 0.3342709565510947334, 52.96022202444907379, 78.69601584788405546 ) ) ;
#13573 = VECTOR ( 'NONE', #12735, 1000.000000000000000 ) ;
#13574 = CARTESIAN_POINT ( 'NONE',  ( 2.436687528221644694, 49.84925249003585179, 69.23980501161587142 ) ) ;
#13575 = ORIENTED_EDGE ( 'NONE', *, *, #14976, .F. ) ;
#13576 = VERTEX_POINT ( 'NONE', #10223 ) ;
#13577 = CARTESIAN_POINT ( 'NONE',  ( 3.959183846440533117, 36.72216061236609619, 76.69403369658814995 ) ) ;
#13578 = VECTOR ( 'NONE', #17635, 1000.000000000000000 ) ;
#13579 = VERTEX_POINT ( 'NONE', #5517 ) ;
#13580 = FACE_OUTER_BOUND ( 'NONE', #15734, .T. ) ;
#13581 = CARTESIAN_POINT ( 'NONE',  ( 0.3332767407100286627, 52.96756894666060589, 77.72734411258261389 ) ) ;
#13582 = CARTESIAN_POINT ( 'NONE',  ( -2.416137431568557314, 39.07291177436112406, 96.27371380123797451 ) ) ;
#13583 = CARTESIAN_POINT ( 'NONE',  ( -3.353456363966241138, 52.20858450364031000, 76.50206692849373269 ) ) ;
#13584 = ORIENTED_EDGE ( 'NONE', *, *, #19498, .T. ) ;
#13585 = AXIS2_PLACEMENT_3D ( 'NONE', #14444, #4743, #9677 ) ;
#13586 = CARTESIAN_POINT ( 'NONE',  ( -1.077846259693497677, 49.76218137147969856, 85.55433879953100984 ) ) ;
#13587 = ORIENTED_EDGE ( 'NONE', *, *, #16909, .F. ) ;
#13588 = LINE ( 'NONE', #10423, #11498 ) ;
#13589 = EDGE_CURVE ( 'NONE', #12459, #11489, #9587, .T. ) ;
#13590 = PLANE ( 'NONE',  #21026 ) ;
#13591 = LINE ( 'NONE', #3904, #13469 ) ;
#13592 = CARTESIAN_POINT ( 'NONE',  ( 8.378637954445377289, 41.81363803720061867, 76.38301527011910252 ) ) ;
#13593 = CARTESIAN_POINT ( 'NONE',  ( 7.680032241523795378, 40.16158449578585277, 77.69330938776616335 ) ) ;
#13594 = DIRECTION ( 'NONE',  ( 0.8043570849667761591, -0.5941461771851692664, 1.733862608106489734E-17 ) ) ;
#13595 = AXIS2_PLACEMENT_3D ( 'NONE', #6704, #1331, #20781 ) ;
#13596 = CARTESIAN_POINT ( 'NONE',  ( 0.6366586698427276758, 52.96517666865470630, 77.38563349023446847 ) ) ;
#13598 = B_SPLINE_CURVE_WITH_KNOTS ( 'NONE', 3,
 ( #11361, #4530, #3160, #6330, #16245, #1666, #17829, #3259, #9446, #11047, #20693, #1460 ),
 .UNSPECIFIED., .F., .F.,
 ( 4, 2, 2, 2, 2, 4 ),
 ( 0.000000000000000000, 0.0001730768718649229035, 0.0003461537437298458069, 0.0004326921796623278043, 0.0005192306155948099100, 0.0006923074874598105508 ),
 .UNSPECIFIED. ) ;
#13597 = VECTOR ( 'NONE', #6745, 1000.000000000000000 ) ;
#13599 = CARTESIAN_POINT ( 'NONE',  ( -4.032264951078912141, 50.98107207184723677, 76.47051527011910821 ) ) ;
#13600 = FACE_OUTER_BOUND ( 'NONE', #8913, .T. ) ;
#13601 = CARTESIAN_POINT ( 'NONE',  ( -2.077846259693550746, 39.65884927180063357, 95.72683880294496817 ) ) ;
#13602 = AXIS2_PLACEMENT_3D ( 'NONE', #8941, #13504, #19208 ) ;
#13603 = CARTESIAN_POINT ( 'NONE',  ( -7.951966518800452022, 41.76130995793021583, 78.71972396713441356 ) ) ;
#13604 = VERTEX_POINT ( 'NONE', #16903 ) ;
#13605 = CARTESIAN_POINT ( 'NONE',  ( 0.3568559529620515813, 52.35602931952836059, 76.07436980028356288 ) ) ;
#13606 = ORIENTED_EDGE ( 'NONE', *, *, #4564, .T. ) ;
#13607 = DIRECTION ( 'NONE',  ( 0.5813877811927011807, -0.8136266022444372803, -5.636455622144619183E-17 ) ) ;
#13608 = CARTESIAN_POINT ( 'NONE',  ( 2.722153740306497927, 51.36218137147969287, 54.55433879953099563 ) ) ;
#13609 = CARTESIAN_POINT ( 'NONE',  ( 24.52215374030649642, 44.16218137147969003, 105.5543387995310098 ) ) ;
#13610 = CARTESIAN_POINT ( 'NONE',  ( 3.460444912181559474, 49.25145096859824889, 93.14871380123798872 ) ) ;
#13611 = AXIS2_PLACEMENT_3D ( 'NONE', #14962, #15173, #19538 ) ;
#13612 = CARTESIAN_POINT ( 'NONE',  ( 30.92220646078100188, 42.76218137147968434, 62.80715055817104542 ) ) ;
#13613 = CARTESIAN_POINT ( 'NONE',  ( -7.474077239038335208, 48.01569385150226310, 78.79824701870994375 ) ) ;
#13614 = ADVANCED_FACE ( 'NONE', ( #13496 ), #4017, .T. ) ;
#13615 = CARTESIAN_POINT ( 'NONE',  ( -2.313335635445065375, 50.56218137147968861, 96.05433879953096721 ) ) ;
#13616 = B_SPLINE_CURVE_WITH_KNOTS ( 'NONE', 3,
 ( #19753, #3685, #16886, #20172, #20063, #16576, #15298, #10521, #18169, #10204 ),
 .UNSPECIFIED., .F., .F.,
 ( 4, 2, 2, 2, 4 ),
 ( 0.000000000000000000, 0.0001230216279879512049, 0.0002460432559759024099, 0.0003690648839638536148, 0.0004920865119518048197 ),
 .UNSPECIFIED. ) ;
#13617 = ORIENTED_EDGE ( 'NONE', *, *, #12169, .T. ) ;
#13618 = VERTEX_POINT ( 'NONE', #8822 ) ;
#13619 = CARTESIAN_POINT ( 'NONE',  ( 8.176702304275824673, 41.66423807893649212, 79.54795956895829079 ) ) ;
#13620 = DIRECTION ( 'NONE',  ( 0.000000000000000000, -1.000000000000000000, 0.000000000000000000 ) ) ;
#13621 = LINE ( 'NONE', #7119, #19439 ) ;
#13622 = VERTEX_POINT ( 'NONE', #730 ) ;
#13623 = CARTESIAN_POINT ( 'NONE',  ( -1.677846259693499542, 50.36218137147968577, 50.15433879953098995 ) ) ;
#13624 = CARTESIAN_POINT ( 'NONE',  ( -4.615672533236396369, 45.70859455045284392, 95.05433879953100984 ) ) ;
#13625 = CARTESIAN_POINT ( 'NONE',  ( 27.63948732994508006, 43.16218137147969003, 76.90433879953101837 ) ) ;
#13626 = CARTESIAN_POINT ( 'NONE',  ( -2.904223097202481174, 48.62752260303690122, 91.58621380294496817 ) ) ;
#13627 = PRODUCT_DEFINITION_FORMATION_WITH_SPECIFIED_SOURCE ( 'ANY', '', #13807, .NOT_KNOWN. ) ;
#13628 = CARTESIAN_POINT ( 'NONE',  ( -7.850119897725965856, 41.43929802982232502, 78.93401657524854897 ) ) ;
#13629 = EDGE_CURVE ( 'NONE', #14920, #6478, #9597, .T. ) ;
#13630 = CARTESIAN_POINT ( 'NONE',  ( -7.640244526827991045, 47.49833189654476939, 78.29855163726114142 ) ) ;
#13631 = CARTESIAN_POINT ( 'NONE',  ( -3.350035803220276609, 49.20851703305431357, 90.88308880123797451 ) ) ;
#13632 = CARTESIAN_POINT ( 'NONE',  ( 6.872381782841294751, 37.88404961645574076, 76.32925572521180868 ) ) ;
#13633 = ORIENTED_EDGE ( 'NONE', *, *, #14976, .T. ) ;
#13634 = CARTESIAN_POINT ( 'NONE',  ( 0.5221537403065019678, 44.16218137147968292, 72.45433879953087342 ) ) ;
#13635 = B_SPLINE_CURVE_WITH_KNOTS ( 'NONE', 3,
 ( #9453, #15939, #7851, #20280, #2744, #12217, #15735, #20395, #5826, #17212 ),
 .UNSPECIFIED., .F., .F.,
 ( 4, 2, 2, 2, 4 ),
 ( 0.000000000000000000, 0.0001356155976497246129, 0.0002712311952994492258, 0.0004068467929491738659, 0.0005424623905988984517 ),
 .UNSPECIFIED. ) ;
#13636 = VERTEX_POINT ( 'NONE', #15422 ) ;
#13637 = CIRCLE ( 'NONE', #10255, 4.200000000000001066 ) ;
#13638 = CARTESIAN_POINT ( 'NONE',  ( -4.302529968709936981, 50.78349582127268746, 78.93463708245236887 ) ) ;
#13639 = AXIS2_PLACEMENT_3D ( 'NONE', #12234, #10228, #3920 ) ;
#13640 = CARTESIAN_POINT ( 'NONE',  ( 6.102441102155617969, 43.42752260303680600, 94.86746380294499659 ) ) ;
#13641 =( BOUNDED_CURVE ( )  B_SPLINE_CURVE ( 3, ( #5441, #771, #4055, #2160 ),
 .UNSPECIFIED., .F., .T. ) 
 B_SPLINE_CURVE_WITH_KNOTS ( ( 4, 4 ),
 ( 2.801755744135676629, 3.481429563043918485 ),
 .UNSPECIFIED. ) 
 CURVE ( )  GEOMETRIC_REPRESENTATION_ITEM ( )  RATIONAL_B_SPLINE_CURVE ( ( 1.000000000000000000, 0.9618726943880423486, 0.9618726943880423486, 1.000000000000000000 ) ) 
 REPRESENTATION_ITEM ( '' )  );
#13642 = ORIENTED_EDGE ( 'NONE', *, *, #17552, .T. ) ;
#13643 = EDGE_CURVE ( 'NONE', #11174, #16680, #7323, .T. ) ;
#13644 = CARTESIAN_POINT ( 'NONE',  ( 2.091368541865482822, 52.21063245889818916, 75.45433879953088763 ) ) ;
#13645 = EDGE_CURVE ( 'NONE', #10593, #10468, #15024, .T. ) ;
#13646 = DIRECTION ( 'NONE',  ( 1.540237394707284220E-16, 1.793354297423764243E-16, -1.000000000000000000 ) ) ;
#13647 = CARTESIAN_POINT ( 'NONE',  ( -5.769203958596529347, 48.43638519259696551, 72.45433879953087342 ) ) ;
#13648 = CARTESIAN_POINT ( 'NONE',  ( -5.368445182934975968, 51.36218137147968577, 45.55433879953098852 ) ) ;
#13649 = CARTESIAN_POINT ( 'NONE',  ( 0.8436899295658937259, 52.35217759412554983, 76.26682227151283655 ) ) ;
#13650 = CARTESIAN_POINT ( 'NONE',  ( 0.3313075116511031704, 52.35623069211510483, 78.62228161321135644 ) ) ;
#13651 = ORIENTED_EDGE ( 'NONE', *, *, #11701, .T. ) ;
#13652 = CARTESIAN_POINT ( 'NONE',  ( 0.5221537403065019678, 44.16218137147968292, 72.45433879953087342 ) ) ;
#13653 = ORIENTED_EDGE ( 'NONE', *, *, #8324, .T. ) ;
#13654 = CARTESIAN_POINT ( 'NONE',  ( 0.5221537403065009686, 44.16218137147968292, 79.45433879953087342 ) ) ;
#13655 = CARTESIAN_POINT ( 'NONE',  ( -7.131166555022944387, 41.64504215559904310, 76.30903472146037814 ) ) ;
#13656 = EDGE_CURVE ( 'NONE', #8316, #2898, #13673, .T. ) ;
#13657 = CARTESIAN_POINT ( 'NONE',  ( -7.355728065240099589, 40.24014096896499382, 77.93115699112124162 ) ) ;
#13658 = AXIS2_PLACEMENT_3D ( 'NONE', #1772, #6427, #4934 ) ;
#13659 = CARTESIAN_POINT ( 'NONE',  ( 2.921181103050038530, 49.30691215337508737, 93.50121379782399345 ) ) ;
#13660 = CARTESIAN_POINT ( 'NONE',  ( -5.841826873769421447, 37.92258288932846710, 75.85972562479176418 ) ) ;
#13661 = VECTOR ( 'NONE', #8143, 1000.000000000000000 ) ;
#13662 = CARTESIAN_POINT ( 'NONE',  ( -4.157721234522135489, 51.63388627315737267, 75.40660817806873695 ) ) ;
#13663 = VERTEX_POINT ( 'NONE', #5292 ) ;
#13664 = DIRECTION ( 'NONE',  ( -1.000000000000000000, 0.000000000000000000, -0.000000000000000000 ) ) ;
#13665 = ORIENTED_EDGE ( 'NONE', *, *, #18419, .T. ) ;
#13666 = CARTESIAN_POINT ( 'NONE',  ( 2.228068668033876154, 49.81017696809242778, 83.28180655319408743 ) ) ;
#13667 = CARTESIAN_POINT ( 'NONE',  ( 3.948530577815480225, 39.69684013992245752, 91.89871379953099506 ) ) ;
#13668 = CARTESIAN_POINT ( 'NONE',  ( -2.904223097202481174, 48.62752260303690122, 96.27371379953099506 ) ) ;
#13669 = ORIENTED_EDGE ( 'NONE', *, *, #9915, .F. ) ;
#13670 = CARTESIAN_POINT ( 'NONE',  ( 3.460444912181559474, 49.25145096859824889, 95.64871380123798872 ) ) ;
#13671 = CARTESIAN_POINT ( 'NONE',  ( 0.3340858135836293763, 52.96017298819928243, 77.67332619259997273 ) ) ;
#13672 = EDGE_LOOP ( 'NONE', ( #14323, #865, #9177, #20144 ) ) ;
#13673 = CIRCLE ( 'NONE', #6521, 3.999999999999996447 ) ;
#13674 = PLANE ( 'NONE',  #9814 ) ;
#13675 = DIRECTION ( 'NONE',  ( 0.007885122365278605591, 0.9999689119394085113, 1.805443505845548073E-16 ) ) ;
#13676 = EDGE_CURVE ( 'NONE', #122, #6553, #2124, .T. ) ;
#13677 = VECTOR ( 'NONE', #3617, 1000.000000000000000 ) ;
#13678 = ORIENTED_EDGE ( 'NONE', *, *, #11215, .T. ) ;
#13679 = CARTESIAN_POINT ( 'NONE',  ( -3.055718635266669647, 36.78391400955043622, 76.62933879953087057 ) ) ;
#13680 = CARTESIAN_POINT ( 'NONE',  ( -5.154188915835984375, 42.64120994080404614, 93.61746380123797451 ) ) ;
#13681 = EDGE_LOOP ( 'NONE', ( #12479, #7477, #483, #9309 ) ) ;
#13682 = DIRECTION ( 'NONE',  ( 1.000000000000000000, 0.000000000000000000, 0.000000000000000000 ) ) ;
#13683 = EDGE_CURVE ( 'NONE', #20489, #10089, #20188, .T. ) ;
#13684 = CARTESIAN_POINT ( 'NONE',  ( 5.611423337425062385, 41.22389019960463230, 90.17996380123798872 ) ) ;
#13685 = EDGE_CURVE ( 'NONE', #11711, #12006, #8623, .T. ) ;
#13686 = CARTESIAN_POINT ( 'NONE',  ( -4.861758623289528458, 37.19864595225625692, 76.03818239474222196 ) ) ;
#13687 = DIRECTION ( 'NONE',  ( -1.540237394707284220E-16, -1.793354297423764243E-16, 1.000000000000000000 ) ) ;
#13688 = VECTOR ( 'NONE', #13823, 1000.000000000000114 ) ;
#13689 = DIRECTION ( 'NONE',  ( -0.2999031954727373050, -0.9539696396349525154, -2.172727669310459771E-16 ) ) ;
#13690 = AXIS2_PLACEMENT_3D ( 'NONE', #7329, #2446, #10865 ) ;
#13691 = ORIENTED_EDGE ( 'NONE', *, *, #11215, .F. ) ;
#13692 = ORIENTED_EDGE ( 'NONE', *, *, #14297, .F. ) ;
#13693 = CARTESIAN_POINT ( 'NONE',  ( 0.6361344075657290320, 52.21317904296746093, 75.36071969156348871 ) ) ;
#13694 = ORIENTED_EDGE ( 'NONE', *, *, #14297, .T. ) ;
#13695 = LINE ( 'NONE', #10634, #19360 ) ;
#13696 = CARTESIAN_POINT ( 'NONE',  ( 0.4711897470839793711, 52.35512766633201664, 77.40025757944940210 ) ) ;
#13697 = FACE_OUTER_BOUND ( 'NONE', #6128, .T. ) ;
#13698 = VERTEX_POINT ( 'NONE', #10756 ) ;
#13699 = CARTESIAN_POINT ( 'NONE',  ( -5.616286711741430793, 44.43019146960381960, 93.73558879782397923 ) ) ;
#13700 = CARTESIAN_POINT ( 'NONE',  ( 6.907457231639352102, 50.38602950313908480, 78.73390793106847241 ) ) ;
#13701 = VERTEX_POINT ( 'NONE', #12228 ) ;
#13702 = PLANE ( 'NONE',  #596 ) ;
#13703 = CARTESIAN_POINT ( 'NONE',  ( -1.477846259693496922, 49.81903562097207327, 51.21119304902337888 ) ) ;
#13704 = CARTESIAN_POINT ( 'NONE',  ( 9.009194133669925719, 41.79485085341455886, 75.38196330830126612 ) ) ;
#13705 = CARTESIAN_POINT ( 'NONE',  ( 0.3821786226492927541, 35.36301154328572949, 76.16022115247204738 ) ) ;
#13706 = DIRECTION ( 'NONE',  ( -1.779391786395883536E-16, -5.922860397471805611E-17, 1.000000000000000000 ) ) ;
#13707 = EDGE_CURVE ( 'NONE', #8776, #799, #10650, .T. ) ;
#13708 = CARTESIAN_POINT ( 'NONE',  ( 4.394343283833276992, 39.11584570990505938, 95.25808880123800293 ) ) ;
#13709 = CARTESIAN_POINT ( 'NONE',  ( 0.8188518330924889899, 52.96374000860539155, 77.51877209028926075 ) ) ;
#13710 = DIRECTION ( 'NONE',  ( -1.779391786395883536E-16, -5.922860397471805611E-17, 1.000000000000000000 ) ) ;
#13711 = CARTESIAN_POINT ( 'NONE',  ( 5.750640099535992533, 51.24052371918730842, 75.36022115247205022 ) ) ;
#13712 = CARTESIAN_POINT ( 'NONE',  ( -3.943187491250720544, 40.73580453397070755, 91.89871380294498238 ) ) ;
#13713 = DIRECTION ( 'NONE',  ( 1.084202172485505420E-16, 1.000000000000000000, 0.000000000000000000 ) ) ;
#13714 = CARTESIAN_POINT ( 'NONE',  ( 8.374959273921817271, 41.81408433146208381, 78.54183882225588320 ) ) ;
#13715 = VECTOR ( 'NONE', #1861, 1000.000000000000000 ) ;
#13716 = ORIENTED_EDGE ( 'NONE', *, *, #18701, .F. ) ;
#13717 = CARTESIAN_POINT ( 'NONE',  ( -4.517176205512259735, 36.94411680087065974, 76.50360254650976799 ) ) ;
#13718 = DIRECTION ( 'NONE',  ( -1.540237394707284467E-16, -1.793354297423764243E-16, 1.000000000000000000 ) ) ;
#13719 = CARTESIAN_POINT ( 'NONE',  ( -4.471346911670678992, 51.40978084683593607, 79.54642512701808243 ) ) ;
#13720 = CARTESIAN_POINT ( 'NONE',  ( -2.416137431568557314, 39.07291177436112406, 96.27371380123797451 ) ) ;
#13721 = CARTESIAN_POINT ( 'NONE',  ( -5.018595066975969132, 37.31449471545010965, 77.33253961758860839 ) ) ;
#13722 = CARTESIAN_POINT ( 'NONE',  ( -5.389245695702297390, 49.84508174962770255, 72.45433879953087342 ) ) ;
#13723 = CARTESIAN_POINT ( 'NONE',  ( -0.7268458593731772499, 40.36218137147969287, 105.5543387995310098 ) ) ;
#13724 = EDGE_CURVE ( 'NONE', #8370, #20695, #4547, .T. ) ;
#13725 = CARTESIAN_POINT ( 'NONE',  ( 5.534705324965363715, 50.64691056217811393, 78.12411320240556734 ) ) ;
#13726 = ORIENTED_EDGE ( 'NONE', *, *, #18570, .F. ) ;
#13727 = EDGE_LOOP ( 'NONE', ( #19973, #15239, #3472, #6332, #2569 ) ) ;
#13728 = CARTESIAN_POINT ( 'NONE',  ( 6.224138097561578320, 50.05597543161009355, 77.64680307551286376 ) ) ;
#13729 = CARTESIAN_POINT ( 'NONE',  ( -4.509672285278093717, 36.93857395727003023, 75.36838243422435824 ) ) ;
#13730 = LINE ( 'NONE', #15654, #17747 ) ;
#13731 = CARTESIAN_POINT ( 'NONE',  ( -3.416655834670953684, 49.09312775377990334, 94.63736517561592620 ) ) ;
#13732 = CARTESIAN_POINT ( 'NONE',  ( -6.782631326057146026, 43.38225751353197523, 78.28007409364852265 ) ) ;
#13733 = DIRECTION ( 'NONE',  ( 1.540237394707284220E-16, 1.793354297423764243E-16, -1.000000000000000000 ) ) ;
#13734 = CARTESIAN_POINT ( 'NONE',  ( -3.943187491250720544, 40.73580453397070755, 93.14871380294496817 ) ) ;
#13735 = CARTESIAN_POINT ( 'NONE',  ( -4.392497846706504561, 51.46612350181082007, 76.19049300047602458 ) ) ;
#13736 = CARTESIAN_POINT ( 'NONE',  ( -3.545047478496396565, 36.22604446995779170, 78.23707788297487298 ) ) ;
#13737 = CARTESIAN_POINT ( 'NONE',  ( -7.724133150439582707, 47.24691236978577535, 78.01104965316210382 ) ) ;
#13738 = CARTESIAN_POINT ( 'NONE',  ( -0.3080929418689875576, 37.85583172076933778, 91.19558880123798872 ) ) ;
#13739 = EDGE_CURVE ( 'NONE', #4812, #11233, #18918, .T. ) ;
#13740 = CARTESIAN_POINT ( 'NONE',  ( 30.92220646078100188, 42.96218137147968008, 58.20715055817105110 ) ) ;
#13741 = VERTEX_POINT ( 'NONE', #20819 ) ;
#13742 = CARTESIAN_POINT ( 'NONE',  ( 1.973315136850091855, 52.23284655848411973, 75.87673665581081650 ) ) ;
#13743 = ORIENTED_EDGE ( 'NONE', *, *, #2976, .F. ) ;
#13744 = CARTESIAN_POINT ( 'NONE',  ( -7.677846259693480668, 36.96218137147968008, 45.55433879953098852 ) ) ;
#13745 = CARTESIAN_POINT ( 'NONE',  ( 5.568489401881125289, 48.03437091500646261, 90.41433880123798872 ) ) ;
#13746 = EDGE_LOOP ( 'NONE', ( #5570, #1458, #12680, #2995 ) ) ;
#13747 = CARTESIAN_POINT ( 'NONE',  ( 0.2541436421823703440, 38.02374091943176637, 94.20433879782399345 ) ) ;
#13748 = CARTESIAN_POINT ( 'NONE',  ( -1.590937568396970203, 39.63064243629642647, 94.82933879953097289 ) ) ;
#13749 = EDGE_CURVE ( 'NONE', #11138, #8211, #14229, .T. ) ;
#13750 = CARTESIAN_POINT ( 'NONE',  ( -2.928118925487932067, 51.59273948230099904, 78.48078762820125576 ) ) ;
#13751 = PLANE ( 'NONE',  #16917 ) ;
#13752 = CARTESIAN_POINT ( 'NONE',  ( 0.5424873107736979394, 52.36227596382597227, 77.38586826841044797 ) ) ;
#13753 = DIRECTION ( 'NONE',  ( -3.211742425186504723E-16, 5.922860397471811774E-17, -1.000000000000000000 ) ) ;
#13754 = ORIENTED_EDGE ( 'NONE', *, *, #10160, .F. ) ;
#13755 = FACE_OUTER_BOUND ( 'NONE', #10576, .T. ) ;
#13756 = ORIENTED_EDGE ( 'NONE', *, *, #8497, .T. ) ;
#13757 = CARTESIAN_POINT ( 'NONE',  ( 4.903891431458001549, 51.86598285117960216, 77.64500276804245971 ) ) ;
#13758 = CARTESIAN_POINT ( 'NONE',  ( 6.786106954071964736, 50.47566606489075980, 77.50555814853646552 ) ) ;
#13759 = DIRECTION ( 'NONE',  ( 1.000000000000000000, -0.000000000000000000, -0.000000000000000000 ) ) ;
#13760 = CARTESIAN_POINT ( 'NONE',  ( 6.811311454328823345, 50.45704851585021800, 79.04700635913849283 ) ) ;
#13761 = DIRECTION ( 'NONE',  ( -1.110223024625156540E-16, -1.000000000000000000, -5.922860397471808077E-17 ) ) ;
#13762 = CARTESIAN_POINT ( 'NONE',  ( 0.2541436421823703440, 38.02374091943176637, 94.20433879782400766 ) ) ;
#13763 = CARTESIAN_POINT ( 'NONE',  ( 5.547036553094518929, 37.68180603056410405, 78.36773547936199691 ) ) ;
#13764 = B_SPLINE_SURFACE_WITH_KNOTS ( 'NONE', 3, 1, ( 
 ( #16601, #16182 ),
 ( #3513, #308 ),
 ( #18190, #2022 ),
 ( #19882, #6908 ),
 ( #19466, #6482 ),
 ( #8519, #15004 ),
 ( #17979, #6586 ),
 ( #11404, #424 ),
 ( #4883, #5302 ),
 ( #16398, #13198 ),
 ( #9703, #3404 ) ),
 .UNSPECIFIED., .F., .F., .F.,
 ( 4, 1, 1, 1, 1, 1, 1, 1, 4 ),
 ( 2, 2 ),
 ( 0.000000000000000000, 0.1891742793480645779, 0.3478164846204494509, 0.4767017694705349973, 0.5812052966572537338, 0.6755649002106222101, 0.7721207368275812000, 0.8786749842102796748, 1.000000000000000000 ),
 ( 0.000000000000000000, 1.000000000000000000 ),
 .UNSPECIFIED. ) ;
#13765 = ORIENTED_EDGE ( 'NONE', *, *, #2105, .T. ) ;
#13766 = CARTESIAN_POINT ( 'NONE',  ( 8.788011242024287739, 41.13195169557157271, 78.55826321071354812 ) ) ;
#13767 =( BOUNDED_CURVE ( )  B_SPLINE_CURVE ( 3, ( #15843, #4444, #6344, #19025 ),
 .UNSPECIFIED., .F., .F. ) 
 B_SPLINE_CURVE_WITH_KNOTS ( ( 4, 4 ),
 ( 1.425105721489102084, 1.727008346339851785 ),
 .UNSPECIFIED. ) 
 CURVE ( )  GEOMETRIC_REPRESENTATION_ITEM ( )  RATIONAL_B_SPLINE_CURVE ( ( 1.000000000000000000, 0.9924189787924448947, 0.9924189787924448947, 1.000000000000000000 ) ) 
 REPRESENTATION_ITEM ( '' )  );
#13768 = ORIENTED_EDGE ( 'NONE', *, *, #10271, .F. ) ;
#13769 = DIRECTION ( 'NONE',  ( 1.779391786395883536E-16, 5.922860397471806844E-17, -1.000000000000000000 ) ) ;
#13770 = CARTESIAN_POINT ( 'NONE',  ( 5.025485839985549319, 41.56218137147963887, 95.72683879953099506 ) ) ;
#13771 = ORIENTED_EDGE ( 'NONE', *, *, #3745, .F. ) ;
#13772 = CARTESIAN_POINT ( 'NONE',  ( 5.611423337425062385, 41.22389019960463230, 92.83621380123797451 ) ) ;
#13773 = CARTESIAN_POINT ( 'NONE',  ( -4.617530944194691678, 50.38537608977133431, 79.48628414162533318 ) ) ;
#13774 = LINE ( 'NONE', #2284, #6870 ) ;
#13775 = CARTESIAN_POINT ( 'NONE',  ( -0.7270676699343749938, 38.96968808794299122, 95.05433879953099563 ) ) ;
#13776 = DIRECTION ( 'NONE',  ( 1.110223024625156417E-16, 1.000000000000000000, 5.922860397471808077E-17 ) ) ;
#13777 = ORIENTED_EDGE ( 'NONE', *, *, #10529, .F. ) ;
#13778 = CARTESIAN_POINT ( 'NONE',  ( 2.096812674726597603, 52.20958845481697352, 78.66304280023771867 ) ) ;
#13779 = CARTESIAN_POINT ( 'NONE',  ( -4.567115856812060670, 47.10047254335474065, 93.46121380123797451 ) ) ;
#13780 = EDGE_LOOP ( 'NONE', ( #14186, #14741, #3714, #3539 ) ) ;
#13781 = CARTESIAN_POINT ( 'NONE',  ( -4.225462782839600528, 50.84799750334796187, 79.54845644658969661 ) ) ;
#13782 = DIRECTION ( 'NONE',  ( 0.000000000000000000, -2.891205793294680792E-16, -1.000000000000000000 ) ) ;
#13783 = PRODUCT_CONTEXT ( 'NONE', #13207, 'mechanical' ) ;
#13784 = CARTESIAN_POINT ( 'NONE',  ( -6.613032277150674432, 45.52591812603678534, 79.45433879953087342 ) ) ;
#13786 = EDGE_CURVE ( 'NONE', #13663, #4828, #4334, .T. ) ;
#13785 = CARTESIAN_POINT ( 'NONE',  ( 1.403788643848842055, 39.16218137147969003, 93.70233169107481785 ) ) ;
#13787 = LINE ( 'NONE', #20376, #6856 ) ;
#13788 = ADVANCED_FACE ( 'NONE', ( #11062 ), #17221, .F. ) ;
#13789 = ORIENTED_EDGE ( 'NONE', *, *, #4402, .F. ) ;
#13790 = LINE ( 'NONE', #12007, #7453 ) ;
#13791 = ORIENTED_EDGE ( 'NONE', *, *, #3004, .F. ) ;
#13792 = CARTESIAN_POINT ( 'NONE',  ( 5.859131993956401274, 51.16038512709904040, 75.36137945677606353 ) ) ;
#13793 = EDGE_CURVE ( 'NONE', #15854, #12698, #6293, .T. ) ;
#13794 = DIRECTION ( 'NONE',  ( 0.007885122365275663500, 0.9999689119394085113, 1.805443505845543142E-16 ) ) ;
#13795 = CARTESIAN_POINT ( 'NONE',  ( 6.198496396448986090, 45.68315280215533392, 91.74246380123798872 ) ) ;
#13796 = EDGE_CURVE ( 'NONE', #6021, #14506, #15689, .T. ) ;
#13797 = EDGE_LOOP ( 'NONE', ( #4572, #7504, #18773, #18152 ) ) ;
#13798 = CARTESIAN_POINT ( 'NONE',  ( 6.030765343457317407, 50.11959148040762102, 79.40187404227555135 ) ) ;
#13799 = ORIENTED_EDGE ( 'NONE', *, *, #1731, .F. ) ;
#13800 = DIRECTION ( 'NONE',  ( 3.211742425186504723E-16, -5.922860397471811774E-17, 1.000000000000000000 ) ) ;
#13801 = DIRECTION ( 'NONE',  ( -5.626130192357176673E-16, -1.831515347669941892E-30, 1.000000000000000000 ) ) ;
#13802 = CARTESIAN_POINT ( 'NONE',  ( 2.635245049009970586, 48.69372030666295359, 90.45433879953097289 ) ) ;
#13803 = CARTESIAN_POINT ( 'NONE',  ( 8.121917471046002035, 44.10225444150351137, 72.45432679953087529 ) ) ;
#13804 = DIRECTION ( 'NONE',  ( -0.000000000000000000, -0.000000000000000000, -1.000000000000000000 ) ) ;
#13805 = DIRECTION ( 'NONE',  ( 5.731934358295347564E-32, -3.469446951953617147E-16, -1.000000000000000000 ) ) ;
#13806 = CARTESIAN_POINT ( 'NONE',  ( 31.07218010054375412, 45.56218137147968861, 64.80574467885102763 ) ) ;
#13807 = PRODUCT ( 'MAS-160', 'MAS-160', '', ( #2517 ) ) ;
#13808 = CARTESIAN_POINT ( 'NONE',  ( 8.849350546267242379, 41.31578948168061061, 75.97436175383765544 ) ) ;
#13809 = CARTESIAN_POINT ( 'NONE',  ( -5.283659240720997019, 50.82933219714914230, 75.48294376282896678 ) ) ;
#13810 = CARTESIAN_POINT ( 'NONE',  ( 4.717386066067114747, 51.07891390471289128, 75.44114465464750197 ) ) ;
#13811 = CARTESIAN_POINT ( 'NONE',  ( 4.987494971863720927, 47.58855820898865829, 91.27371380294496817 ) ) ;
#13812 = CARTESIAN_POINT ( 'NONE',  ( 5.722153740306500147, 44.16218137147969003, 77.84651775085080772 ) ) ;
#13813 = ORIENTED_EDGE ( 'NONE', *, *, #14769, .T. ) ;
#13814 = CARTESIAN_POINT ( 'NONE',  ( 8.912702722122396892, 41.50565997170561161, 78.91042349786003740 ) ) ;
#13815 = AXIS2_PLACEMENT_3D ( 'NONE', #1828, #8313, #4994 ) ;
#13816 = ORIENTED_EDGE ( 'NONE', *, *, #5988, .F. ) ;
#13817 = CARTESIAN_POINT ( 'NONE',  ( -7.367656984315424928, 48.05973018190410073, 72.45433879953087342 ) ) ;
#13818 = LINE ( 'NONE', #15212, #18083 ) ;
#13819 = EDGE_CURVE ( 'NONE', #17272, #8211, #14389, .T. ) ;
#13820 = CARTESIAN_POINT ( 'NONE',  ( -3.477340361660131496, 52.12006153457090818, 79.00686454089694166 ) ) ;
#13821 = CARTESIAN_POINT ( 'NONE',  ( 4.394343283833276992, 39.11584570990505938, 95.25808880123800293 ) ) ;
#13822 = DIRECTION ( 'NONE',  ( -1.334402673828310381E-16, -2.168404344970984413E-15, 1.000000000000000000 ) ) ;
#13823 = DIRECTION ( 'NONE',  ( -0.5773502691896219563, 0.5773502691896226224, -0.5773502691896327255 ) ) ;
#13824 = CARTESIAN_POINT ( 'NONE',  ( 8.571241826522742357, 42.59017791465015534, 78.02841696848460629 ) ) ;
#13825 = CARTESIAN_POINT ( 'NONE',  ( 8.951667845840693971, 41.62244091939069790, 76.38301527011910252 ) ) ;
#13826 = ORIENTED_EDGE ( 'NONE', *, *, #2173, .T. ) ;
#13827 = ORIENTED_EDGE ( 'NONE', *, *, #3619, .F. ) ;
#13828 = PRODUCT_DEFINITION_CONTEXT ( 'detailed design', #14284, 'design' ) ;
#13829 = CARTESIAN_POINT ( 'NONE',  ( 6.291655274237696993, 49.98965726174421320, 77.59820540376455256 ) ) ;
#13830 = DIRECTION ( 'NONE',  ( 3.154042683594179442E-15, -3.469446951953613203E-16, -1.000000000000000000 ) ) ;
#13831 = CARTESIAN_POINT ( 'NONE',  ( 30.92220646078100188, 45.56218137147968861, 56.80715055817104542 ) ) ;
#13832 = CARTESIAN_POINT ( 'NONE',  ( 10.77494014480653917, 42.96218137147968008, 61.40715055817103263 ) ) ;
#13833 = CARTESIAN_POINT ( 'NONE',  ( -3.582310441719081417, 40.15725564764044009, 95.05433879953096721 ) ) ;
#13834 = CARTESIAN_POINT ( 'NONE',  ( 9.178784097065811665, 42.30312273229867515, 78.05372954401303787 ) ) ;
#13835 = CARTESIAN_POINT ( 'NONE',  ( 5.025485839985549319, 41.56218137147963887, 89.78933880294498238 ) ) ;
#13836 = CARTESIAN_POINT ( 'NONE',  ( -4.404666252920439895, 51.45742840424412634, 76.10127045261064893 ) ) ;
#13837 = CARTESIAN_POINT ( 'NONE',  ( -7.727295065384001127, 47.23743591010920539, 77.61879955032603107 ) ) ;
#13838 = CARTESIAN_POINT ( 'NONE',  ( -5.954796862783082290, 38.00602926950411842, 78.58503192925951453 ) ) ;
#13839 = CARTESIAN_POINT ( 'NONE',  ( -8.191933259318233240, 42.93552377858928537, 78.37203949479768994 ) ) ;
#13840 = EDGE_LOOP ( 'NONE', ( #6694, #14321, #12318, #15041, #12213, #1694, #16107, #20689, #16728, #2311, #13527 ) ) ;
#13841 = CARTESIAN_POINT ( 'NONE',  ( 5.894741035747108171, 51.13408216234794423, 77.22227766523002401 ) ) ;
#13842 = ORIENTED_EDGE ( 'NONE', *, *, #16514, .F. ) ;
#13843 = AXIS2_PLACEMENT_3D ( 'NONE', #14437, #4850, #19321 ) ;
#13844 = CARTESIAN_POINT ( 'NONE',  ( -4.804644443005473775, 51.17161863374555963, 78.45066232894264147 ) ) ;
#13845 = CARTESIAN_POINT ( 'NONE',  ( 6.198496396448986090, 45.68315280215533392, 91.58621380123798872 ) ) ;
#13846 = VERTEX_POINT ( 'NONE', #4230 ) ;
#13847 = CARTESIAN_POINT ( 'NONE',  ( -1.477846259693490705, 50.16218137147969713, 61.55433879953100273 ) ) ;
#13848 = LINE ( 'NONE', #10475, #19650 ) ;
#13849 = CARTESIAN_POINT ( 'NONE',  ( -2.915674812773581426, 51.60163158963862173, 78.23748737924660190 ) ) ;
#13850 = LINE ( 'NONE', #19631, #5005 ) ;
#13851 = CARTESIAN_POINT ( 'NONE',  ( 5.710003222748535556, 51.27054054311695808, 77.28795170149270177 ) ) ;
#13852 = CARTESIAN_POINT ( 'NONE',  ( 0.5221537403065114047, 44.16218137147969713, 45.55433879953100273 ) ) ;
#13853 = ORIENTED_EDGE ( 'NONE', *, *, #3280, .F. ) ;
#13854 = CARTESIAN_POINT ( 'NONE',  ( 1.652727357819364418, 35.35299279957455099, 76.86610350541323555 ) ) ;
#13855 = EDGE_CURVE ( 'NONE', #15529, #6294, #9146, .T. ) ;
#13856 = VECTOR ( 'NONE', #10026, 1000.000000000000000 ) ;
#13857 = ORIENTED_EDGE ( 'NONE', *, *, #11341, .F. ) ;
#13858 = CARTESIAN_POINT ( 'NONE',  ( -0.8071739151948656987, 40.17810205696807913, 82.45433879953087342 ) ) ;
#13859 = DIRECTION ( 'NONE',  ( 1.334402673828313339E-16, 1.871524341742854397E-32, -1.000000000000000000 ) ) ;
#13860 = LINE ( 'NONE', #18650, #16927 ) ;
#13861 = DIRECTION ( 'NONE',  ( -1.779391786395883536E-16, -5.922860397471806844E-17, 1.000000000000000000 ) ) ;
#13862 = CARTESIAN_POINT ( 'NONE',  ( 0.5221537403065015237, 44.16218137147968292, 75.45433879953088763 ) ) ;
#13863 = B_SPLINE_CURVE_WITH_KNOTS ( 'NONE', 3,
 ( #5888, #5662, #988, #7478, #18763, #5981, #20930, #16071, #11287, #3085, #9585, #12385 ),
 .UNSPECIFIED., .F., .F.,
 ( 4, 2, 2, 2, 2, 4 ),
 ( 0.000000000000000000, 0.0005742104900236383314, 0.001148420980047276663, 0.001435526225059106887, 0.001722631470070937545, 0.002296841960094558530 ),
 .UNSPECIFIED. ) ;
#13864 = CARTESIAN_POINT ( 'NONE',  ( 5.856396280011939126, 46.10368687828906076, 94.59496379782397923 ) ) ;
#13865 = CARTESIAN_POINT ( 'NONE',  ( -6.782631326057146026, 43.38225751353197523, 78.13669174070733447 ) ) ;
#13866 = ORIENTED_EDGE ( 'NONE', *, *, #16583, .F. ) ;
#13867 = CARTESIAN_POINT ( 'NONE',  ( 4.311926990668543347, 51.43403001777136296, 77.50896141901741032 ) ) ;
#13868 = AXIS2_PLACEMENT_3D ( 'NONE', #6476, #11500, #6682 ) ;
#13869 = ORIENTED_EDGE ( 'NONE', *, *, #16018, .F. ) ;
#13870 = LINE ( 'NONE', #10606, #3066 ) ;
#13871 = CARTESIAN_POINT ( 'NONE',  ( 5.025485839985549319, 41.56218137147963887, 91.97683879953100927 ) ) ;
#13872 = CARTESIAN_POINT ( 'NONE',  ( -7.275583942264174375, 42.06582416155776372, 77.46376836651262465 ) ) ;
#13873 = ORIENTED_EDGE ( 'NONE', *, *, #19181, .F. ) ;
#13874 = CARTESIAN_POINT ( 'NONE',  ( -4.524181921268124462, 40.28999182795290324, 92.44558880123798872 ) ) ;
#13875 = DIRECTION ( 'NONE',  ( 0.9480563259966822143, 0.3181025035073955509, 2.030702297275135124E-16 ) ) ;
#13876 = CARTESIAN_POINT ( 'NONE',  ( -4.567115856812060670, 47.10047254335474065, 94.55496380123807398 ) ) ;
#13877 = ORIENTED_EDGE ( 'NONE', *, *, #17837, .T. ) ;
#13878 = DIRECTION ( 'NONE',  ( 1.000000000000000000, 1.402518428993842030E-16, 3.154042683594179047E-15 ) ) ;
#13879 = PLANE ( 'NONE',  #3710 ) ;
#13880 = ORIENTED_EDGE ( 'NONE', *, *, #12150, .F. ) ;
#13881 = FACE_BOUND ( 'NONE', #16238, .T. ) ;
#13882 = CARTESIAN_POINT ( 'NONE',  ( 0.7561398222055120133, 52.96423844662842129, 78.87878230117789258 ) ) ;
#13883 = EDGE_CURVE ( 'NONE', #16412, #10206, #7649, .T. ) ;
#13884 = VERTEX_POINT ( 'NONE', #19028 ) ;
#13885 = CARTESIAN_POINT ( 'NONE',  ( 2.722153740306517911, 47.73989013547934945, 56.15433879953099705 ) ) ;
#13886 = DIRECTION ( 'NONE',  ( 6.308085367188358884E-15, 8.847205979147994320E-31, 1.000000000000000000 ) ) ;
#13887 =( REPRESENTATION_RELATIONSHIP ('NONE','NONE', #11365, #7678 ) REPRESENTATION_RELATIONSHIP_WITH_TRANSFORMATION ( #9115 )SHAPE_REPRESENTATION_RELATIONSHIP( ) );
#13888 = VECTOR ( 'NONE', #10707, 1000.000000000000000 ) ;
#13889 = CARTESIAN_POINT ( 'NONE',  ( 5.427780505986066650, 36.85179043424346190, 76.70433879953087342 ) ) ;
#13890 = CARTESIAN_POINT ( 'NONE',  ( 5.449567083428624947, 36.86735832482640518, 76.18683980367092090 ) ) ;
#13891 = DIRECTION ( 'NONE',  ( 1.540237394707284220E-16, 1.793354297423764243E-16, -1.000000000000000000 ) ) ;
#13892 = EDGE_CURVE ( 'NONE', #8376, #9419, #4445, .T. ) ;
#13893 = EDGE_LOOP ( 'NONE', ( #17833, #548, #20996, #10846 ) ) ;
#13894 = CARTESIAN_POINT ( 'NONE',  ( 1.288664704385863669, 52.20803360176820007, 75.43490186719157009 ) ) ;
#13895 = EDGE_CURVE ( 'NONE', #14061, #12858, #9358, .T. ) ;
#13896 = VERTEX_POINT ( 'NONE', #12650 ) ;
#13897 = CARTESIAN_POINT ( 'NONE',  ( 6.645808250425207397, 50.57929906569810896, 75.61685692759286326 ) ) ;
#13898 = CARTESIAN_POINT ( 'NONE',  ( 27.03948732994508930, 43.16218137147969003, 76.90433879953101837 ) ) ;
#13899 = CARTESIAN_POINT ( 'NONE',  ( -5.784195910403845176, 44.99242805365518194, 91.03933880123798872 ) ) ;
#13900 = CARTESIAN_POINT ( 'NONE',  ( -3.350440871817599753, 52.21073926392551812, 76.59793576264409865 ) ) ;
#13901 = ORIENTED_EDGE ( 'NONE', *, *, #10649, .T. ) ;
#13902 = VECTOR ( 'NONE', #19782, 1000.000000000000114 ) ;
#13903 = ADVANCED_FACE ( 'NONE', ( #17744 ), #10249, .F. ) ;
#13904 = CARTESIAN_POINT ( 'NONE',  ( -4.461854692652708287, 50.67442117498146104, 75.36473603976158131 ) ) ;
#13905 = ORIENTED_EDGE ( 'NONE', *, *, #14455, .T. ) ;
#13906 = PLANE ( 'NONE',  #15910 ) ;
#13907 = EDGE_CURVE ( 'NONE', #5223, #11489, #19640, .T. ) ;
#13908 = DIRECTION ( 'NONE',  ( 1.540237394707284220E-16, 1.793354297423764243E-16, -1.000000000000000000 ) ) ;
#13909 = CARTESIAN_POINT ( 'NONE',  ( 7.686881228206692285, 40.21297994929685160, 76.12035193564865665 ) ) ;
#13910 = EDGE_CURVE ( 'NONE', #10028, #2112, #13066, .T. ) ;
#13911 = AXIS2_PLACEMENT_3D ( 'NONE', #826, #929, #3902 ) ;
#13912 = CARTESIAN_POINT ( 'NONE',  ( 6.184266552044742404, 50.09404646486822088, 75.56305138714441227 ) ) ;
#13913 = PLANE ( 'NONE',  #12830 ) ;
#13914 = CARTESIAN_POINT ( 'NONE',  ( 3.178197289651383262, 41.22014870947117515, 98.25514354869233102 ) ) ;
#13915 = CARTESIAN_POINT ( 'NONE',  ( 1.352400422481993658, 50.46853102219002096, 95.72683880123798872 ) ) ;
#13916 = DIRECTION ( 'NONE',  ( -1.540237394707284220E-16, -1.793354297423764243E-16, 1.000000000000000000 ) ) ;
#13917 = VECTOR ( 'NONE', #12816, 1000.000000000000000 ) ;
#13918 = CARTESIAN_POINT ( 'NONE',  ( -5.134411146083727395, 50.01620383897704869, 75.69846806870741318 ) ) ;
#13919 = CARTESIAN_POINT ( 'NONE',  ( 5.531249400824703955, 51.40257879072892422, 75.36789977960694387 ) ) ;
#13920 = EDGE_CURVE ( 'NONE', #6135, #12999, #5065, .T. ) ;
#13921 = CARTESIAN_POINT ( 'NONE',  ( 4.987494971863720927, 47.58855820898865829, 95.02371380294496817 ) ) ;
#13922 = AXIS2_PLACEMENT_3D ( 'NONE', #10863, #15642, #14034 ) ;
#13923 = CARTESIAN_POINT ( 'NONE',  ( -4.257991192395801150, 43.33247370687232092, 79.04308574771191331 ) ) ;
#13924 = ORIENTED_EDGE ( 'NONE', *, *, #12095, .F. ) ;
#13925 = CARTESIAN_POINT ( 'NONE',  ( 8.865792162213244509, 41.36506604770743678, 78.93669174070734584 ) ) ;
#13926 = VECTOR ( 'NONE', #9299, 1000.000000000000000 ) ;
#13927 = DIRECTION ( 'NONE',  ( -1.540237394707284220E-16, -1.793354297423764243E-16, 1.000000000000000000 ) ) ;
#13928 = VECTOR ( 'NONE', #10487, 1000.000000000000000 ) ;
#13929 = CARTESIAN_POINT ( 'NONE',  ( 23.03948732994508575, 45.16218137147969003, 76.90433879953101837 ) ) ;
#13930 = CARTESIAN_POINT ( 'NONE',  ( 31.22215374030650281, 42.96218137147968008, 77.40433879953098995 ) ) ;
#13931 = CARTESIAN_POINT ( 'NONE',  ( 11.22215374030650281, 45.56218137147968150, 72.80433879953100984 ) ) ;
#13932 = CARTESIAN_POINT ( 'NONE',  ( -4.861758623289527570, 37.19864595225625692, 76.03818239474222196 ) ) ;
#13933 = CARTESIAN_POINT ( 'NONE',  ( -7.606686202760679194, 43.11990846545297273, 78.43041451606663372 ) ) ;
#13934 = CARTESIAN_POINT ( 'NONE',  ( 8.638503602126267111, 42.99341659656273862, 77.63357130927565208 ) ) ;
#13935 = AXIS2_PLACEMENT_3D ( 'NONE', #17598, #17706, #16120 ) ;
#13936 = ORIENTED_EDGE ( 'NONE', *, *, #15889, .T. ) ;
#13937 = VERTEX_POINT ( 'NONE', #19226 ) ;
#13938 = VECTOR ( 'NONE', #13769, 1000.000000000000000 ) ;
#13939 = CARTESIAN_POINT ( 'NONE',  ( -4.385124331863694991, 37.59250281884201428, 78.93547643519214319 ) ) ;
#13941 = ADVANCED_FACE ( 'NONE', ( #17847 ), #4957, .T. ) ;
#13940 = LINE ( 'NONE', #8949, #15546 ) ;
#13942 = CARTESIAN_POINT ( 'NONE',  ( 8.896031707678503153, 41.45569588382780779, 75.98771331677210128 ) ) ;
#13943 = CARTESIAN_POINT ( 'NONE',  ( 5.929557977968517690, 51.10836428964097422, 77.10005730845655592 ) ) ;
#13944 = B_SPLINE_SURFACE_WITH_KNOTS ( 'NONE', 3, 1, ( 
 ( #10349, #853 ),
 ( #10453, #13619 ),
 ( #15333, #20095 ),
 ( #13509, #15119 ),
 ( #16820, #8639 ),
 ( #19986, #7117 ),
 ( #10671, #3717 ),
 ( #10238, #5307 ),
 ( #5413, #2138 ),
 ( #6913, #431 ),
 ( #15223, #12140 ),
 ( #2238, #16919 ),
 ( #5533, #18619 ),
 ( #12040, #15436 ),
 ( #2343, #746 ),
 ( #4033, #8948 ),
 ( #7230, #10559 ),
 ( #7337, #20307 ),
 ( #5737, #12247 ),
 ( #18729, #4142 ),
 ( #2029, #13416 ),
 ( #19887, #2769 ),
 ( #15652, #17447 ),
 ( #14357, #9270 ),
 ( #20421, #2966 ),
 ( #1067, #17541 ),
 ( #14241, #2872 ) ),
 .UNSPECIFIED., .F., .F., .F.,
 ( 4, 1, 1, 1, 1, 1, 1, 1, 1, 1, 1, 1, 1, 1, 1, 1, 1, 1, 1, 1, 1, 1, 1, 1, 4 ),
 ( 2, 2 ),
 ( 0.000000000000000000, 0.06037445285962812075, 0.1180910611743953287, 0.1732658017268006723, 0.2259310541736886668, 0.2758310469819637567, 0.3235430165773793276, 0.3690552752481174870, 0.4126046436208182233, 0.4542408720228611196, 0.4938267050212239995, 0.5316899362873784840, 0.5681969051958857264, 0.6035856803598054210, 0.6378784996589128564, 0.6713567270158068423, 0.7043713979572046036, 0.7376082755227613141, 0.7714571943499641815, 0.8061103333465380327, 0.8420729482554840661, 0.8794516251380997129, 0.9177737848194706949, 0.9579350591099196066, 1.000000000000000000 ),
 ( 0.000000000000000000, 1.000000000000000000 ),
 .UNSPECIFIED. ) ;
#13945 = CARTESIAN_POINT ( 'NONE',  ( 8.951218635964366399, 41.62109460889399770, 77.24172240072661566 ) ) ;
#13946 = VECTOR ( 'NONE', #10119, 1000.000000000000000 ) ;
#13947 = CARTESIAN_POINT ( 'NONE',  ( 9.201306621205869618, 42.37062416594873326, 78.02362291919803283 ) ) ;
#13948 = CARTESIAN_POINT ( 'NONE',  ( 3.122153740306552905, 48.66551347115873227, 90.10183880294498238 ) ) ;
#13949 = EDGE_CURVE ( 'NONE', #11635, #3380, #4642, .T. ) ;
#13951 = ADVANCED_FACE ( 'NONE', ( #1578 ), #1888, .T. ) ;
#13950 = CARTESIAN_POINT ( 'NONE',  ( -4.448383556050954368, 51.42618962001968441, 76.01002907825849775 ) ) ;
#13952 = CARTESIAN_POINT ( 'NONE',  ( -7.484880448772741168, 47.96396789458968613, 78.32492703482499508 ) ) ;
#13953 = CARTESIAN_POINT ( 'NONE',  ( 5.146043734657006041, 40.41782908280415398, 90.15009084312077903 ) ) ;
#13954 = CARTESIAN_POINT ( 'NONE',  ( 5.722750437672663892, 37.06256514788822898, 75.36130176902827316 ) ) ;
#13955 = VERTEX_POINT ( 'NONE', #1476 ) ;
#13956 = EDGE_CURVE ( 'NONE', #3254, #19301, #9362, .T. ) ;
#13957 = CARTESIAN_POINT ( 'NONE',  ( 0.5221537403065010796, 44.16218137147969003, 77.84651775085080772 ) ) ;
#13958 = ORIENTED_EDGE ( 'NONE', *, *, #14500, .F. ) ;
#13959 = DIRECTION ( 'NONE',  ( 0.000000000000000000, 0.000000000000000000, -1.000000000000000000 ) ) ;
#13960 = CARTESIAN_POINT ( 'NONE',  ( -3.981178359372548492, 46.76218137147973408, 90.41433880294496817 ) ) ;
#13961 = ORIENTED_EDGE ( 'NONE', *, *, #6776, .F. ) ;
#13962 = CARTESIAN_POINT ( 'NONE',  ( -1.219503646467433589, 49.90383875825363447, 77.41268141275706682 ) ) ;
#13963 = LINE ( 'NONE', #978, #8793 ) ;
#13964 = CARTESIAN_POINT ( 'NONE',  ( -4.181418169567056253, 51.61695331097443784, 79.50772166908967620 ) ) ;
#13965 = DIRECTION ( 'NONE',  ( 0.5954989751681698529, -0.8033560671169786005, -5.234922652618075161E-17 ) ) ;
#13966 = DIRECTION ( 'NONE',  ( -1.110223024625156540E-16, -1.000000000000000000, -5.922860397471808077E-17 ) ) ;
#13967 = CARTESIAN_POINT ( 'NONE',  ( -4.473072018670162464, 36.91153881467540288, 79.53329352641277694 ) ) ;
#13968 = ORIENTED_EDGE ( 'NONE', *, *, #15102, .F. ) ;
#13969 = DIRECTION ( 'NONE',  ( -0.9485903129789527988, 0.3165065846431829311, -8.934458285744989980E-17 ) ) ;
#13970 = CARTESIAN_POINT ( 'NONE',  ( -1.419351766502867873, 49.49642391118513274, 93.50121379782397923 ) ) ;
#13971 = EDGE_LOOP ( 'NONE', ( #3134, #1729, #8387, #8110, #16299 ) ) ;
#13972 = CARTESIAN_POINT ( 'NONE',  ( -5.004817973257477348, 39.29348442311233214, 77.05433879953086773 ) ) ;
#13973 = CARTESIAN_POINT ( 'NONE',  ( -5.835824771109036746, 39.98772221508849611, 72.45433879953085921 ) ) ;
#13974 = CARTESIAN_POINT ( 'NONE',  ( 30.92220646078100188, 42.76218137147968434, 61.40715055817103263 ) ) ;
#13975 = FACE_OUTER_BOUND ( 'NONE', #19000, .T. ) ;
#13976 = CARTESIAN_POINT ( 'NONE',  ( 5.841953631609400510, 37.14774338596793513, 76.17246542145134924 ) ) ;
#13977 = CARTESIAN_POINT ( 'NONE',  ( 5.437844490049829282, 37.59859269650263514, 78.34743064351589226 ) ) ;
#13978 = B_SPLINE_CURVE_WITH_KNOTS ( 'NONE', 3,
 ( #21031, #7870, #9788, #8180, #4759, #10979, #11177, #11285, #17543, #6467, #14359 ),
 .UNSPECIFIED., .F., .F.,
 ( 4, 1, 1, 1, 1, 1, 1, 1, 4 ),
 ( 0.000000000000000000, 0.1230989878275519644, 0.2403818709996815850, 0.3547287725962395277, 0.4701889909135318901, 0.5896219003167558759, 0.7153806559642975627, 0.8522030906580475573, 1.000000000000000000 ),
 .UNSPECIFIED. ) ;
#13979 = EDGE_LOOP ( 'NONE', ( #9129, #7023, #17735, #16449 ) ) ;
#13980 = CARTESIAN_POINT ( 'NONE',  ( -0.3916064810627546966, 36.00492801184311986, 78.58487462435995496 ) ) ;
#13981 = VECTOR ( 'NONE', #623, 1000.000000000000000 ) ;
#13982 = VERTEX_POINT ( 'NONE', #19437 ) ;
#13983 = LINE ( 'NONE', #17076, #14616 ) ;
#13984 = CARTESIAN_POINT ( 'NONE',  ( 1.256812508749381774, 49.74246873332880625, 91.11746379953096664 ) ) ;
#13985 = CARTESIAN_POINT ( 'NONE',  ( -7.795419580117447289, 41.25910984028834605, 78.43135113490271237 ) ) ;
#13986 = VERTEX_POINT ( 'NONE', #4855 ) ;
#13987 = CARTESIAN_POINT ( 'NONE',  ( 5.611423337425062385, 41.22389019960463230, 91.58621380123798872 ) ) ;
#13988 = CARTESIAN_POINT ( 'NONE',  ( 3.394637663597737998, 39.16678726411793576, 95.40913173179340845 ) ) ;
#13989 = FACE_BOUND ( 'NONE', #18128, .T. ) ;
#13990 = CARTESIAN_POINT ( 'NONE',  ( 5.035970566151715566, 36.57181739631530348, 75.46362501775257670 ) ) ;
#13991 = CARTESIAN_POINT ( 'NONE',  ( 3.099655065065782367, 37.00631057046152961, 75.45433879953087342 ) ) ;
#13992 = VERTEX_POINT ( 'NONE', #3270 ) ;
#13993 = CARTESIAN_POINT ( 'NONE',  ( 1.034831540439702158, 52.34672676983775119, 79.52523235054587758 ) ) ;
#13994 = CARTESIAN_POINT ( 'NONE',  ( -4.567115856812060670, 47.10047254335474065, 92.21121380123797451 ) ) ;
#13995 = AXIS2_PLACEMENT_3D ( 'NONE', #15648, #3925, #5629 ) ;
#13996 = ORIENTED_EDGE ( 'NONE', *, *, #13270, .T. ) ;
#13997 = PLANE ( 'NONE',  #20259 ) ;
#13998 = CARTESIAN_POINT ( 'NONE',  ( -0.2058114043728421494, 41.98042365162810086, 80.45433879953087342 ) ) ;
#13999 = VECTOR ( 'NONE', #14037, 1000.000000000000114 ) ;
#14000 = CARTESIAN_POINT ( 'NONE',  ( 5.666884522201896424, 41.76315400873614436, 91.93871379782397923 ) ) ;
#14001 = CARTESIAN_POINT ( 'NONE',  ( 5.196215417279978155, 37.43323793221333773, 75.99415254657458263 ) ) ;
#14002 = CARTESIAN_POINT ( 'NONE',  ( 5.628424039023946612, 51.33079979992434261, 78.86786983087660019 ) ) ;
#14003 = CARTESIAN_POINT ( 'NONE',  ( 31.22215374030650281, 42.96218137147968008, 77.40433879953098995 ) ) ;
#14004 = ORIENTED_EDGE ( 'NONE', *, *, #529, .F. ) ;
#14005 = EDGE_CURVE ( 'NONE', #11406, #7250, #2802, .T. ) ;
#14006 = CARTESIAN_POINT ( 'NONE',  ( 1.832302049357034335, 52.95658493274570588, 75.70482343270806780 ) ) ;
#14007 = EDGE_LOOP ( 'NONE', ( #20272, #11398, #20237, #14070 ) ) ;
#14008 = VECTOR ( 'NONE', #1058, 1000.000000000000000 ) ;
#14009 = CARTESIAN_POINT ( 'NONE',  ( -0.7686299002591694407, 52.26036095920864000, 79.04667360578667967 ) ) ;
#14010 = CARTESIAN_POINT ( 'NONE',  ( 0.5312634811787118050, 52.96600774845068571, 77.38663191694250543 ) ) ;
#14011 = CARTESIAN_POINT ( 'NONE',  ( 4.394343283833276992, 39.11584570990505938, 95.10183880123797451 ) ) ;
#14012 = CIRCLE ( 'NONE', #2458, 4.199999999999999289 ) ;
#14013 = EDGE_LOOP ( 'NONE', ( #11892, #9218, #3417, #15403, #15272 ) ) ;
#14014 = CARTESIAN_POINT ( 'NONE',  ( -4.609362567131230826, 46.70091906356311995, 92.45433879953098710 ) ) ;
#14015 = EDGE_LOOP ( 'NONE', ( #13127, #17875, #14405, #8946 ) ) ;
#14016 = CARTESIAN_POINT ( 'NONE',  ( 5.196643236000038080, 51.64973888592641771, 79.48101422306089603 ) ) ;
#14017 = CARTESIAN_POINT ( 'NONE',  ( 31.07218010054375412, 42.96218137147968008, 66.20574467885104752 ) ) ;
#14018 = CARTESIAN_POINT ( 'NONE',  ( -1.187946976321870629, 48.86064447540922373, 90.61058879953097289 ) ) ;
#14019 = EDGE_CURVE ( 'NONE', #3927, #1640, #17316, .T. ) ;
#14020 = ORIENTED_EDGE ( 'NONE', *, *, #11853, .F. ) ;
#14021 = FACE_OUTER_BOUND ( 'NONE', #17087, .T. ) ;
#14022 = DIRECTION ( 'NONE',  ( -1.110223024625156540E-16, -1.000000000000000000, -5.922860397471808077E-17 ) ) ;
#14023 = CARTESIAN_POINT ( 'NONE',  ( -7.611239903938034068, 43.11915264683222659, 78.37207201143637292 ) ) ;
#14024 = CARTESIAN_POINT ( 'NONE',  ( -2.416137431568557314, 39.07291177436112406, 91.27371380123798872 ) ) ;
#14025 = PLANE ( 'NONE',  #17922 ) ;
#14026 =( BOUNDED_CURVE ( )  B_SPLINE_CURVE ( 2, ( #15425, #2443, #12442, #12544, #5622 ),
 .UNSPECIFIED., .F., .F. ) 
 B_SPLINE_CURVE_WITH_KNOTS ( ( 3, 2, 3 ),
 ( 0.1128933701044576160, 0.1302041294069655186, 0.1389341928972610829 ),
 .UNSPECIFIED. ) 
 CURVE ( )  GEOMETRIC_REPRESENTATION_ITEM ( )  RATIONAL_B_SPLINE_CURVE ( ( 0.9660722070856899713, 0.9493985675917875344, 1.000000000000000000, 0.9744809739478270671, 0.9660722130355270387 ) ) 
 REPRESENTATION_ITEM ( '' )  );
#14027 = CARTESIAN_POINT ( 'NONE',  ( -4.567115856812060670, 47.10047254335474065, 92.05496380123798872 ) ) ;
#14028 = VECTOR ( 'NONE', #13120, 1000.000000000000000 ) ;
#14029 = DIRECTION ( 'NONE',  ( -1.110223024625156540E-16, -1.000000000000000000, -5.922860397471808077E-17 ) ) ;
#14030 = CARTESIAN_POINT ( 'NONE',  ( -2.904223097202481174, 48.62752260303690122, 90.33621380294496817 ) ) ;
#14031 = ADVANCED_FACE ( 'NONE', ( #13376 ), #18161, .T. ) ;
#14032 = CARTESIAN_POINT ( 'NONE',  ( -7.290527651941959952, 40.11224193202943411, 78.50801527011910252 ) ) ;
#14033 = CARTESIAN_POINT ( 'NONE',  ( 8.375193797766709025, 41.81478721430313072, 78.41904468188381827 ) ) ;
#14034 = DIRECTION ( 'NONE',  ( -0.3165065846431826535, -0.9485903129789529098, -2.188653791613874008E-16 ) ) ;
#14035 = LINE ( 'NONE', #12656, #8908 ) ;
#14036 = CARTESIAN_POINT ( 'NONE',  ( 8.385768451058924100, 39.92640453324153071, 77.75090705316073070 ) ) ;
#14037 = DIRECTION ( 'NONE',  ( -0.9485903129789527988, 0.3165065846431829311, -8.934458285744989980E-17 ) ) ;
#14038 = CIRCLE ( 'NONE', #2501, 6.200000000000000178 ) ;
#14039 = CARTESIAN_POINT ( 'NONE',  ( -7.811913822204808788, 47.00317617979911944, 79.21909685159604919 ) ) ;
#14040 = FACE_OUTER_BOUND ( 'NONE', #9828, .T. ) ;
#14041 = ORIENTED_EDGE ( 'NONE', *, *, #9856, .F. ) ;
#14042 = CARTESIAN_POINT ( 'NONE',  ( 0.5221537403064990812, 44.16218137147969003, 95.05433879953096721 ) ) ;
#14043 = DIRECTION ( 'NONE',  ( 0.9996789974703350623, -0.02533578529877749536, 1.494306935163130398E-16 ) ) ;
#14044 = LINE ( 'NONE', #17029, #5855 ) ;
#14045 = DIRECTION ( 'NONE',  ( 1.084202172485505420E-16, 1.000000000000000000, 0.000000000000000000 ) ) ;
#14046 = CARTESIAN_POINT ( 'NONE',  ( 5.388356174074294458, 50.75501278463794819, 77.94845644658968808 ) ) ;
#14047 = PLANE ( 'NONE',  #11246 ) ;
#14048 = PLANE ( 'NONE',  #15569 ) ;
#14049 = CARTESIAN_POINT ( 'NONE',  ( 10.77494014480653561, 42.76218137147968434, 77.80433879953099563 ) ) ;
#14050 = AXIS2_PLACEMENT_3D ( 'NONE', #3082, #17345, #9583 ) ;
#14051 = CARTESIAN_POINT ( 'NONE',  ( 1.352400422481993658, 50.46853102219002096, 91.82058880123801714 ) ) ;
#14052 = EDGE_CURVE ( 'NONE', #12950, #10787, #6871, .T. ) ;
#14053 = DIRECTION ( 'NONE',  ( -1.779391786395883783E-16, -5.922860397471806844E-17, 1.000000000000000000 ) ) ;
#14054 = ORIENTED_EDGE ( 'NONE', *, *, #14734, .F. ) ;
#14055 = EDGE_CURVE ( 'NONE', #11467, #9723, #16676, .T. ) ;
#14056 = CARTESIAN_POINT ( 'NONE',  ( 0.5221537403065005245, 44.16218137147968292, 82.45433879953087342 ) ) ;
#14057 = EDGE_LOOP ( 'NONE', ( #17171, #18069, #8418, #9326 ) ) ;
#14058 = DIRECTION ( 'NONE',  ( 0.000000000000000000, 0.000000000000000000, 1.000000000000000000 ) ) ;
#14059 = EDGE_CURVE ( 'NONE', #18295, #8403, #19943, .T. ) ;
#14060 = CARTESIAN_POINT ( 'NONE',  ( -4.500660556396669065, 42.81632233694663370, 93.07058880294496817 ) ) ;
#14061 = VERTEX_POINT ( 'NONE', #15076 ) ;
#14062 = CARTESIAN_POINT ( 'NONE',  ( 5.856396280011939126, 46.10368687828906076, 94.59496379782397923 ) ) ;
#14063 = EDGE_CURVE ( 'NONE', #19757, #2342, #14356, .T. ) ;
#14064 = VECTOR ( 'NONE', #1519, 1000.000000000000000 ) ;
#14065 = CARTESIAN_POINT ( 'NONE',  ( -0.9375041090292165480, 52.97865058173552910, 77.15777051809955367 ) ) ;
#14066 = FACE_OUTER_BOUND ( 'NONE', #5603, .T. ) ;
#14067 = LINE ( 'NONE', #12684, #12795 ) ;
#14068 = DIRECTION ( 'NONE',  ( -0.8146038580541393737, 0.5800177190770224867, -2.145060549591027246E-17 ) ) ;
#14069 = CARTESIAN_POINT ( 'NONE',  ( 2.522153740306492864, 49.81903562097208749, 51.21119304902340019 ) ) ;
#14070 = ORIENTED_EDGE ( 'NONE', *, *, #7699, .F. ) ;
#14071 = ADVANCED_FACE ( 'NONE', ( #708 ), #8912, .T. ) ;
#14072 = FACE_OUTER_BOUND ( 'NONE', #20495, .T. ) ;
#14073 = EDGE_LOOP ( 'NONE', ( #5362, #12181, #4077, #15008, #15678, #15107, #16063, #18969 ) ) ;
#14074 = CARTESIAN_POINT ( 'NONE',  ( 6.153536035488349043, 50.12267912296926653, 77.68963291717793140 ) ) ;
#14075 = CARTESIAN_POINT ( 'NONE',  ( 4.728442938187240152, 51.99557958566231264, 77.51131257087278925 ) ) ;
#14076 = FACE_OUTER_BOUND ( 'NONE', #15291, .T. ) ;
#14077 = CARTESIAN_POINT ( 'NONE',  ( 0.5221537403065040772, 39.16218137147969003, 94.91636871766883132 ) ) ;
#14078 = LINE ( 'NONE', #12589, #14222 ) ;
#14079 = CARTESIAN_POINT ( 'NONE',  ( -1.419351766502868761, 49.49642391118513274, 94.90746379782397923 ) ) ;
#14080 = CARTESIAN_POINT ( 'NONE',  ( -5.338436749040042173, 37.55074888198200256, 75.45005776384208218 ) ) ;
#14081 = VERTEX_POINT ( 'NONE', #18578 ) ;
#14082 = CARTESIAN_POINT ( 'NONE',  ( 2.927603783594689979, 51.37146775011972011, 72.45432679953087529 ) ) ;
#14083 = VERTEX_POINT ( 'NONE', #11782 ) ;
#14084 = LINE ( 'NONE', #20568, #18348 ) ;
#14085 = EDGE_CURVE ( 'NONE', #8218, #16809, #758, .T. ) ;
#14086 = CARTESIAN_POINT ( 'NONE',  ( 5.611423337425062385, 41.22389019960463230, 92.83621380123797451 ) ) ;
#14087 = CARTESIAN_POINT ( 'NONE',  ( 5.750640099535992533, 51.24052371918730842, 75.36022115247205022 ) ) ;
#14088 = ORIENTED_EDGE ( 'NONE', *, *, #6710, .T. ) ;
#14089 = CARTESIAN_POINT ( 'NONE',  ( -4.888424451833091489, 50.19180550725726420, 79.37256909934775706 ) ) ;
#14090 = CARTESIAN_POINT ( 'NONE',  ( 4.178421596892070156, 40.17206517740157778, 93.50121379611698558 ) ) ;
#14092 = CARTESIAN_POINT ( 'NONE',  ( 4.442698562174268062, 36.14788694334743013, 76.14998054923410109 ) ) ;
#14091 = B_SPLINE_CURVE_WITH_KNOTS ( 'NONE', 3,
 ( #10253, #18112, #3533, #10037 ),
 .UNSPECIFIED., .F., .F.,
 ( 4, 4 ),
 ( 0.01428392225856177540, 0.01552286970674648242 ),
 .UNSPECIFIED. ) ;
#14093 = CARTESIAN_POINT ( 'NONE',  ( 0.2965220188279399371, 38.27753855637592295, 95.05433879953093879 ) ) ;
#14094 = VERTEX_POINT ( 'NONE', #2196 ) ;
#14095 = CARTESIAN_POINT ( 'NONE',  ( -4.574316323987747346, 51.33620267474496757, 79.54845644658969661 ) ) ;
#14096 = CARTESIAN_POINT ( 'NONE',  ( 0.6316246594797694236, 52.96522029444659552, 78.93480014378108933 ) ) ;
#14097 = ORIENTED_EDGE ( 'NONE', *, *, #11826, .T. ) ;
#14098 = CARTESIAN_POINT ( 'NONE',  ( -0.05336403213008323460, 39.08435147610357774, 92.45433879953100131 ) ) ;
#14099 = CARTESIAN_POINT ( 'NONE',  ( 4.134898411747151670, 47.90306806511021875, 95.05422504033560926 ) ) ;
#14100 = CARTESIAN_POINT ( 'NONE',  ( 5.052198367669454626, 48.31320248322254685, 93.42308879782400766 ) ) ;
#14101 = ITEM_DEFINED_TRANSFORMATION ( 'NONE', 'NONE', #15663,  #18366 ) ;
#14102 = CARTESIAN_POINT ( 'NONE',  ( 5.096251760688711663, 37.36180756311627960, 76.18683980367092090 ) ) ;
#14103 = CARTESIAN_POINT ( 'NONE',  ( 8.798005484913860030, 41.16190507553456968, 76.10950202369875228 ) ) ;
#14104 = CARTESIAN_POINT ( 'NONE',  ( -5.462576778579502523, 43.73439565840071452, 80.45433879953087342 ) ) ;
#14105 = ORIENTED_EDGE ( 'NONE', *, *, #20743, .T. ) ;
#14106 = CARTESIAN_POINT ( 'NONE',  ( -7.153763766568051352, 47.04667285769743046, 77.69611589407060137 ) ) ;
#14107 = ORIENTED_EDGE ( 'NONE', *, *, #8841, .F. ) ;
#14108 = CARTESIAN_POINT ( 'NONE',  ( 5.787513446439723985, 51.21328686317854562, 75.36061482756318242 ) ) ;
#14109 = LINE ( 'NONE', #17721, #16037 ) ;
#14110 = CARTESIAN_POINT ( 'NONE',  ( 5.568489401881125289, 48.03437091500646261, 95.41433880123797451 ) ) ;
#14111 = CARTESIAN_POINT ( 'NONE',  ( -3.060074010023764668, 51.53860695331515274, 75.91504661370008478 ) ) ;
#14112 = ORIENTED_EDGE ( 'NONE', *, *, #11853, .T. ) ;
#14113 = ORIENTED_EDGE ( 'NONE', *, *, #8177, .T. ) ;
#14114 = CARTESIAN_POINT ( 'NONE',  ( -4.680892486399498509, 37.06504742266799468, 75.36060488990274564 ) ) ;
#14115 = CYLINDRICAL_SURFACE ( 'NONE', #20487, 0.9921021478795063464 ) ;
#14116 = ORIENTED_EDGE ( 'NONE', *, *, #7260, .F. ) ;
#14117 = CARTESIAN_POINT ( 'NONE',  ( 5.323881593982133786, 50.64173803113061467, 79.54845644658969661 ) ) ;
#14118 = CARTESIAN_POINT ( 'NONE',  ( -7.204754451251679015, 41.41175569818021529, 79.53765352848668613 ) ) ;
#14119 = CARTESIAN_POINT ( 'NONE',  ( 8.509969478268430976, 40.29864289095467456, 75.64968528315669971 ) ) ;
#14120 = ORIENTED_EDGE ( 'NONE', *, *, #19274, .F. ) ;
#14121 = CARTESIAN_POINT ( 'NONE',  ( -4.681776609547195100, 37.06570048882255008, 77.92992558049613194 ) ) ;
#14122 = CARTESIAN_POINT ( 'NONE',  ( 5.869592478971509486, 51.15265838819242106, 78.02050120841747116 ) ) ;
#14123 = CARTESIAN_POINT ( 'NONE',  ( 5.508100443945853186, 47.59510827513957310, 72.45433879953087342 ) ) ;
#14124 = CARTESIAN_POINT ( 'NONE',  ( 6.198496396448986090, 45.68315280215533392, 90.49246380123798872 ) ) ;
#14125 = CARTESIAN_POINT ( 'NONE',  ( -5.368445182934975968, 51.36218137147968577, 93.55433879953098142 ) ) ;
#14126 = ADVANCED_FACE ( 'NONE', ( #5593 ), #12098, .F. ) ;
#14127 = CARTESIAN_POINT ( 'NONE',  ( -0.8237052942265477018, 49.18499566818285018, 94.00808880294498238 ) ) ;
#14128 = DIRECTION ( 'NONE',  ( -0.9485903129789527988, 0.3165065846431829311, -8.934458285744989980E-17 ) ) ;
#14129 = CARTESIAN_POINT ( 'NONE',  ( 8.358012262001102144, 41.76329306163730593, 78.86350455626283917 ) ) ;
#14130 = EDGE_CURVE ( 'NONE', #3211, #9657, #7073, .T. ) ;
#14131 = CARTESIAN_POINT ( 'NONE',  ( -3.638881865703802454, 47.35505628976665804, 92.88950776816830057 ) ) ;
#14132 = FACE_OUTER_BOUND ( 'NONE', #1896, .T. ) ;
#14133 = DIRECTION ( 'NONE',  ( -1.402518428993831183E-16, 1.000000000000000000, -3.469446951953617640E-16 ) ) ;
#14134 = CARTESIAN_POINT ( 'NONE',  ( 5.724311780639353309, 51.25997138778688367, 75.97249762499970416 ) ) ;
#14135 = CARTESIAN_POINT ( 'NONE',  ( 4.394343283833276992, 39.11584570990505938, 91.50808880123798872 ) ) ;
#14136 = CARTESIAN_POINT ( 'NONE',  ( -7.150534706529382056, 46.78250046532827611, 79.21909685159604919 ) ) ;
#14137 = CARTESIAN_POINT ( 'NONE',  ( 8.594421463742152767, 42.71629281084112506, 77.95855867472361922 ) ) ;
#14138 = CARTESIAN_POINT ( 'NONE',  ( 8.215612168451047026, 41.32480612096441064, 78.66873573524837582 ) ) ;
#14139 = CARTESIAN_POINT ( 'NONE',  ( -3.547760446584432348, 36.22804843019941501, 78.70659543854198148 ) ) ;
#14140 = CARTESIAN_POINT ( 'NONE',  ( -6.709328582052545009, 40.29621921162755172, 75.45433879953087342 ) ) ;
#14141 = CARTESIAN_POINT ( 'NONE',  ( -7.423951210289297720, 47.94363824867885171, 78.32492703482499508 ) ) ;
#14142 = DIRECTION ( 'NONE',  ( -1.110223024625156540E-16, -1.000000000000000000, -5.922860397471808077E-17 ) ) ;
#14143 = CARTESIAN_POINT ( 'NONE',  ( 0.5221537403064979710, 39.16218137147969003, 93.35386871425482980 ) ) ;
#14144 = CARTESIAN_POINT ( 'NONE',  ( 11.22215374030649926, 45.56218137147968150, 64.80574467885102763 ) ) ;
#14145 = CIRCLE ( 'NONE', #14485, 6.200000000000000178 ) ;
#14146 = ORIENTED_EDGE ( 'NONE', *, *, #11754, .T. ) ;
#14147 = CARTESIAN_POINT ( 'NONE',  ( -4.524181921268124462, 40.28999182795290324, 92.28933880123798872 ) ) ;
#14148 = EDGE_CURVE ( 'NONE', #16344, #8675, #13472, .T. ) ;
#14149 = CARTESIAN_POINT ( 'NONE',  ( -4.901409867458520253, 51.10247360423972651, 79.52300236340988704 ) ) ;
#14150 = DIRECTION ( 'NONE',  ( 0.000000000000000000, 0.000000000000000000, -1.000000000000000000 ) ) ;
#14151 = EDGE_CURVE ( 'NONE', #16492, #271, #14910, .T. ) ;
#14152 = VERTEX_POINT ( 'NONE', #2299 ) ;
#14153 = DIRECTION ( 'NONE',  ( -0.8043570849667734945, 0.5941461771851728191, -1.733862608106382498E-17 ) ) ;
#14154 = CARTESIAN_POINT ( 'NONE',  ( -2.077846259693550746, 39.65884927180063357, 93.22683880294496817 ) ) ;
#14155 = ORIENTED_EDGE ( 'NONE', *, *, #389, .F. ) ;
#14156 = CARTESIAN_POINT ( 'NONE',  ( -1.419351766502868317, 49.49642391118513274, 93.65746379782397923 ) ) ;
#14157 = CARTESIAN_POINT ( 'NONE',  ( -4.677846259693816400, 43.47758838402643988, 93.98325776475002158 ) ) ;
#14158 = VECTOR ( 'NONE', #18861, 1000.000000000000000 ) ;
#14159 = CARTESIAN_POINT ( 'NONE',  ( -4.451370124631321090, 50.68173085449596726, 76.23059302469468435 ) ) ;
#14160 = LINE ( 'NONE', #20643, #17210 ) ;
#14161 = DIRECTION ( 'NONE',  ( 0.8136266022444381685, 0.5813877811926999595, 2.295812393977108607E-16 ) ) ;
#14162 = DIRECTION ( 'NONE',  ( 1.000000000000000000, 0.000000000000000000, 0.000000000000000000 ) ) ;
#14163 = ORIENTED_EDGE ( 'NONE', *, *, #9013, .F. ) ;
#14164 = EDGE_CURVE ( 'NONE', #3603, #5849, #4992, .T. ) ;
#14165 = CARTESIAN_POINT ( 'NONE',  ( 2.392664886727891460, 47.70104341108812918, 85.28382765310961133 ) ) ;
#14166 = ORIENTED_EDGE ( 'NONE', *, *, #8222, .T. ) ;
#14167 = ADVANCED_FACE ( 'NONE', ( #15819 ), #10834, .T. ) ;
#14168 = CARTESIAN_POINT ( 'NONE',  ( 35.92215374030650565, 40.96218137147972982, 93.55433879953098142 ) ) ;
#14169 = CARTESIAN_POINT ( 'NONE',  ( 10.77494014480653561, 42.96218137147968008, 73.80433879953100984 ) ) ;
#14170 = CARTESIAN_POINT ( 'NONE',  ( -12.18117835937254867, 39.56218137147966019, 53.35433879953099989 ) ) ;
#14171 = CARTESIAN_POINT ( 'NONE',  ( -3.628867371436365730, 48.69222599884265179, 94.98558879782399345 ) ) ;
#14172 = CARTESIAN_POINT ( 'NONE',  ( 34.76745320192721778, 49.36218137147971419, 93.55433879953098142 ) ) ;
#14173 = ADVANCED_FACE ( 'NONE', ( #2724 ), #914, .T. ) ;
#14174 = EDGE_CURVE ( 'NONE', #12584, #4385, #18681, .T. ) ;
#14175 = PRESENTATION_LAYER_ASSIGNMENT (  '', '', ( #11146 ) ) ;
#14176 = VERTEX_POINT ( 'NONE', #17197 ) ;
#14177 = DIRECTION ( 'NONE',  ( 1.540237394707284220E-16, 1.793354297423764243E-16, -1.000000000000000000 ) ) ;
#14178 = EDGE_CURVE ( 'NONE', #10420, #6493, #9228, .T. ) ;
#14179 = EDGE_LOOP ( 'NONE', ( #975, #20453, #18165, #776, #18635, #16547 ) ) ;
#14180 = DIRECTION ( 'NONE',  ( 0.000000000000000000, 0.000000000000000000, -1.000000000000000000 ) ) ;
#14181 = CARTESIAN_POINT ( 'NONE',  ( 3.122153740306552905, 48.66551347115873227, 91.03933879953099506 ) ) ;
#14182 = CARTESIAN_POINT ( 'NONE',  ( 5.333527369480803415, 51.54862809055342154, 75.39573407869305299 ) ) ;
#14183 = EDGE_LOOP ( 'NONE', ( #19833, #11102, #14695, #995 ) ) ;
#14184 = CARTESIAN_POINT ( 'NONE',  ( -4.195629287973702048, 50.68685156650132484, 79.54703672271651271 ) ) ;
#14185 = CARTESIAN_POINT ( 'NONE',  ( -4.677846259693498432, 44.16218137147969003, 93.95661078214054385 ) ) ;
#14186 = ORIENTED_EDGE ( 'NONE', *, *, #947, .T. ) ;
#14187 = VECTOR ( 'NONE', #13295, 1000.000000000000000 ) ;
#14188 = CARTESIAN_POINT ( 'NONE',  ( 6.716472115211415961, 37.77264227618470471, 78.07897440853361104 ) ) ;
#14189 = FACE_OUTER_BOUND ( 'NONE', #7076, .T. ) ;
#14190 = ORIENTED_EDGE ( 'NONE', *, *, #9609, .T. ) ;
#14191 = FACE_OUTER_BOUND ( 'NONE', #11260, .T. ) ;
#14192 = CARTESIAN_POINT ( 'NONE',  ( -5.154188915835984375, 42.64120994080404614, 91.11746380123797451 ) ) ;
#14193 = AXIS2_PLACEMENT_3D ( 'NONE', #4845, #14539, #21003 ) ;
#14194 = ORIENTED_EDGE ( 'NONE', *, *, #11328, .F. ) ;
#14195 = CARTESIAN_POINT ( 'NONE',  ( -5.388909339631083206, 49.84547635099989549, 78.62002338016745284 ) ) ;
#14196 = CARTESIAN_POINT ( 'NONE',  ( 5.519652126588233898, 41.52382328956674939, 95.05433879953105247 ) ) ;
#14197 = EDGE_CURVE ( 'NONE', #13055, #18958, #7623, .T. ) ;
#14198 = SHAPE_REPRESENTATION ( 'Washer', ( #18366 ), #7495 ) ;
#14199 = CARTESIAN_POINT ( 'NONE',  ( 6.660594192354429843, 43.89417127335556046, 93.26683879782399345 ) ) ;
#14200 = CARTESIAN_POINT ( 'NONE',  ( 5.168178938657410626, 37.41320409107064648, 76.01263398532663018 ) ) ;
#14201 = EDGE_CURVE ( 'NONE', #19914, #11768, #13787, .T. ) ;
#14202 = CARTESIAN_POINT ( 'NONE',  ( 5.599886173630381769, 51.35187957151522653, 78.68193220087633222 ) ) ;
#14203 = CIRCLE ( 'NONE', #18960, 0.5999999999999928724 ) ;
#14204 = CARTESIAN_POINT ( 'NONE',  ( -3.310515886049998358, 36.97763837711306678, 77.59103917682324436 ) ) ;
#14205 = ORIENTED_EDGE ( 'NONE', *, *, #8317, .F. ) ;
#14206 = CARTESIAN_POINT ( 'NONE',  ( 2.109887651937126574, 52.20155892434686251, 78.45122513788126639 ) ) ;
#14207 = CARTESIAN_POINT ( 'NONE',  ( -3.936224163802637399, 36.51499092983547001, 77.70026928173652436 ) ) ;
#14208 = ORIENTED_EDGE ( 'NONE', *, *, #4061, .T. ) ;
#14209 = CARTESIAN_POINT ( 'NONE',  ( -1.493738069816088920, 38.45421922485636657, 72.45432679953087529 ) ) ;
#14210 = CARTESIAN_POINT ( 'NONE',  ( 5.649998448837412646, 37.01057924028687296, 77.75931883872233641 ) ) ;
#14211 = CARTESIAN_POINT ( 'NONE',  ( 2.043125170982144745, 38.48583871533720213, 91.42996380123798872 ) ) ;
#14212 = CARTESIAN_POINT ( 'NONE',  ( -4.303670962001103106, 50.79176777958974753, 75.36022115247205022 ) ) ;
#14213 = ORIENTED_EDGE ( 'NONE', *, *, #13276, .T. ) ;
#14214 = ORIENTED_EDGE ( 'NONE', *, *, #9504, .T. ) ;
#14215 = CARTESIAN_POINT ( 'NONE',  ( 23.03948732994508930, 27.61837231449496244, 73.00433879953101268 ) ) ;
#14216 = CARTESIAN_POINT ( 'NONE',  ( -4.185586155588906010, 37.45382053025712565, 76.09208750614521932 ) ) ;
#14217 = CARTESIAN_POINT ( 'NONE',  ( 6.152864644243832615, 50.94341665060460400, 79.51305506302354331 ) ) ;
#14218 = VERTEX_POINT ( 'NONE', #14104 ) ;
#14219 = CARTESIAN_POINT ( 'NONE',  ( 8.648170029844118645, 43.06315486489794608, 77.06316232894263862 ) ) ;
#14220 = CARTESIAN_POINT ( 'NONE',  ( 8.293280423777593668, 41.56926772713645590, 77.52492703482499792 ) ) ;
#14221 = CARTESIAN_POINT ( 'NONE',  ( 29.52548583998564524, 58.44153517398036257, 45.55433879953098852 ) ) ;
#14222 = VECTOR ( 'NONE', #5891, 1000.000000000000227 ) ;
#14223 = ORIENTED_EDGE ( 'NONE', *, *, #5545, .T. ) ;
#14224 = CARTESIAN_POINT ( 'NONE',  ( 6.300200331733075032, 49.98117806904839000, 75.66941908770607483 ) ) ;
#14225 = FILL_AREA_STYLE_COLOUR ( '', #7027 ) ;
#14226 = CARTESIAN_POINT ( 'NONE',  ( 6.293245987533939712, 38.33655849317105435, 75.75804681942297236 ) ) ;
#14227 = CARTESIAN_POINT ( 'NONE',  ( -5.154188915835984375, 42.64120994080404614, 93.61746380123797451 ) ) ;
#14228 = CARTESIAN_POINT ( 'NONE',  ( 5.714504673297025938, 37.81512451739774150, 78.37063972127445766 ) ) ;
#14229 = LINE ( 'NONE', #10860, #3133 ) ;
#14230 = CARTESIAN_POINT ( 'NONE',  ( 5.132218997419849771, 37.56036858369791531, 75.36140480012781495 ) ) ;
#14231 = AXIS2_PLACEMENT_3D ( 'NONE', #2793, #10791, #18954 ) ;
#14232 = CARTESIAN_POINT ( 'NONE',  ( -0.9223007646069696364, 52.21731522718776830, 78.60293901857092180 ) ) ;
#14233 = LINE ( 'NONE', #18922, #3044 ) ;
#14234 = FACE_OUTER_BOUND ( 'NONE', #18514, .T. ) ;
#14235 = CARTESIAN_POINT ( 'NONE',  ( 5.561690527597086486, 51.38009315662554854, 76.32883089164610624 ) ) ;
#14236 = CARTESIAN_POINT ( 'NONE',  ( 2.043125170982144745, 38.48583871533720213, 91.42996380123798872 ) ) ;
#14237 = ORIENTED_EDGE ( 'NONE', *, *, #6506, .T. ) ;
#14238 = CARTESIAN_POINT ( 'NONE',  ( -7.600258659080383339, 43.09958255378303704, 78.69093640348562246 ) ) ;
#14239 = DIRECTION ( 'NONE',  ( 3.893792155548169402E-16, 7.183611964723547524E-17, -1.000000000000000000 ) ) ;
#14240 = ORIENTED_EDGE ( 'NONE', *, *, #5063, .F. ) ;
#14241 = CARTESIAN_POINT ( 'NONE',  ( 9.353817388681445522, 42.82770861117572281, 78.41904468188381827 ) ) ;
#14242 = CARTESIAN_POINT ( 'NONE',  ( -4.074300354217368358, 50.95281676589303999, 76.03497679752658200 ) ) ;
#14243 = CARTESIAN_POINT ( 'NONE',  ( -4.865811501566807529, 37.20163965017977858, 78.83844719616611485 ) ) ;
#14244 = CARTESIAN_POINT ( 'NONE',  ( -0.8237052942265477018, 49.18499566818285018, 91.19558879953099506 ) ) ;
#14245 = CARTESIAN_POINT ( 'NONE',  ( 2.228068668033876154, 49.81017696809242778, 95.05433879953098142 ) ) ;
#14246 = CARTESIAN_POINT ( 'NONE',  ( 5.267397447889379691, 50.84436012315604358, 78.02054163389647101 ) ) ;
#14247 = CARTESIAN_POINT ( 'NONE',  ( 8.643306328402520222, 43.06267994005154520, 77.22643688620827618 ) ) ;
#14248 = FACE_OUTER_BOUND ( 'NONE', #19801, .T. ) ;
#14249 = AXIS2_PLACEMENT_3D ( 'NONE', #6148, #16054, #16157 ) ;
#14250 = CARTESIAN_POINT ( 'NONE',  ( 8.788342534296720743, 41.13294459952883386, 78.64407474691132904 ) ) ;
#14251 = VECTOR ( 'NONE', #4924, 1000.000000000000227 ) ;
#14252 = CARTESIAN_POINT ( 'NONE',  ( -5.323589340698339001, 50.80079960963960417, 79.37256909934775706 ) ) ;
#14253 = EDGE_CURVE ( 'NONE', #895, #7921, #2619, .T. ) ;
#14254 = CARTESIAN_POINT ( 'NONE',  ( -3.135751968098504427, 36.82324114996664122, 77.34971200965068761 ) ) ;
#14255 = VECTOR ( 'NONE', #13371, 1000.000000000000000 ) ;
#14256 = CIRCLE ( 'NONE', #4744, 1.399999999999995026 ) ;
#14257 = VERTEX_POINT ( 'NONE', #5920 ) ;
#14258 = LINE ( 'NONE', #2787, #15313 ) ;
#14259 = CARTESIAN_POINT ( 'NONE',  ( 1.256812508749381774, 49.74246873332880625, 91.42996380294499659 ) ) ;
#14260 = ORIENTED_EDGE ( 'NONE', *, *, #20158, .T. ) ;
#14261 = CARTESIAN_POINT ( 'NONE',  ( 5.887048643069795695, 51.13976422295020541, 78.81551702238962775 ) ) ;
#14263 = AXIS2_PLACEMENT_3D ( 'NONE', #1223, #7814, #15810 ) ;
#14262 = DIRECTION ( 'NONE',  ( -1.540237394707284467E-16, -1.793354297423764243E-16, 1.000000000000000000 ) ) ;
#14264 = CARTESIAN_POINT ( 'NONE',  ( 8.825683451842801119, 41.24485769827808213, 77.95380709400741637 ) ) ;
#14265 = DIRECTION ( 'NONE',  ( -1.000000000000000000, -1.213411507412056509E-16, 0.000000000000000000 ) ) ;
#14266 = CARTESIAN_POINT ( 'NONE',  ( 0.8282905380627915148, 52.35229902398692303, 76.10706146582900544 ) ) ;
#14267 = DIRECTION ( 'NONE',  ( 0.3165065846431827645, 0.9485903129789529098, 0.000000000000000000 ) ) ;
#14268 = EDGE_LOOP ( 'NONE', ( #15923, #13195, #7611, #3333 ) ) ;
#14269 = CARTESIAN_POINT ( 'NONE',  ( 5.824017363460040286, 37.13492678543709502, 77.62670008255557264 ) ) ;
#14270 = ADVANCED_FACE ( 'NONE', ( #17098 ), #20680, .F. ) ;
#14271 = VERTEX_POINT ( 'NONE', #1023 ) ;
#14272 = CARTESIAN_POINT ( 'NONE',  ( 5.568489401881125289, 48.03437091500646261, 94.16433880123797451 ) ) ;
#14273 = VECTOR ( 'NONE', #4148, 1000.000000000000000 ) ;
#14274 = AXIS2_PLACEMENT_3D ( 'NONE', #16836, #15240, #12055 ) ;
#14275 = CARTESIAN_POINT ( 'NONE',  ( -7.261358630300751571, 46.74278378791238708, 79.27428047227293462 ) ) ;
#14276 = CARTESIAN_POINT ( 'NONE',  ( 0.1927955687583305933, 35.96649868655307358, 78.00552566015733191 ) ) ;
#14277 = CARTESIAN_POINT ( 'NONE',  ( 5.760549983993971779, 37.08957531975971023, 75.99604373986946371 ) ) ;
#14278 = FACE_OUTER_BOUND ( 'NONE', #10174, .T. ) ;
#14279 = EDGE_CURVE ( 'NONE', #15007, #7833, #4516, .T. ) ;
#14280 = B_SPLINE_SURFACE_WITH_KNOTS ( 'NONE', 3, 1, ( 
 ( #12644, #14339 ),
 ( #7641, #19220 ),
 ( #11055, #9454 ),
 ( #2536, #7533 ),
 ( #932, #5936 ),
 ( #20396, #19019 ),
 ( #5827, #10749 ),
 ( #12433, #7852 ),
 ( #10953, #1048 ),
 ( #20813, #4325 ),
 ( #17322, #15626 ),
 ( #9031, #7419 ),
 ( #6142, #2949 ),
 ( #20604, #19126 ),
 ( #2745, #9250 ),
 ( #15736, #12331 ),
 ( #18813, #4440 ),
 ( #4223, #17213 ),
 ( #1156, #6032 ) ),
 .UNSPECIFIED., .F., .F., .F.,
 ( 4, 1, 1, 1, 1, 1, 1, 1, 1, 1, 1, 1, 1, 1, 1, 1, 4 ),
 ( 2, 2 ),
 ( 0.000000000000000000, 0.08922172431123952252, 0.1727371540427279917, 0.2514909308953109934, 0.3251734978287333933, 0.3948954482456704107, 0.4603701760623962747, 0.5227882573036246594, 0.5823557395532832359, 0.6395037089141992759, 0.6939186205323212286, 0.7459813003653354979, 0.7965562351082946524, 0.8464932973566897667, 0.8966162271720948818, 0.9474565856282386456, 1.000000000000000000 ),
 ( 0.000000000000000000, 1.000000000000000000 ),
 .UNSPECIFIED. ) ;
#14281 = VECTOR ( 'NONE', #1775, 1000.000000000000000 ) ;
#14282 = ORIENTED_EDGE ( 'NONE', *, *, #19324, .T. ) ;
#14283 = CARTESIAN_POINT ( 'NONE',  ( 4.661266133293011649, 52.04520038539091331, 77.98100106196224601 ) ) ;
#14284 = APPLICATION_CONTEXT ( 'automotive_design' ) ;
#14285 = EDGE_CURVE ( 'NONE', #16046, #20386, #5808, .T. ) ;
#14286 = ADVANCED_FACE ( 'NONE', ( #17298 ), #15344, .F. ) ;
#14287 = ORIENTED_EDGE ( 'NONE', *, *, #15241, .T. ) ;
#14288 = CARTESIAN_POINT ( 'NONE',  ( -3.349945445540459588, 52.21109327740445138, 76.66413924479479647 ) ) ;
#14289 = CARTESIAN_POINT ( 'NONE',  ( -0.9988176903691428077, 49.83852402762217082, 95.80496380123798872 ) ) ;
#14290 = CARTESIAN_POINT ( 'NONE',  ( -7.084928339392615015, 41.46291127039725666, 78.49688471925094291 ) ) ;
#14291 = VERTEX_POINT ( 'NONE', #19514 ) ;
#14292 = FACE_OUTER_BOUND ( 'NONE', #1321, .T. ) ;
#14293 = CARTESIAN_POINT ( 'NONE',  ( -5.060671531193845496, 45.43096853849363725, 95.05433879953096721 ) ) ;
#14294 = VERTEX_POINT ( 'NONE', #3146 ) ;
#14295 = CARTESIAN_POINT ( 'NONE',  ( 4.400857426521584514, 36.11798879971178167, 76.47837415541054895 ) ) ;
#14296 = CARTESIAN_POINT ( 'NONE',  ( 2.916646314871006229, 38.79555996194933698, 95.05433879953095300 ) ) ;
#14297 = EDGE_CURVE ( 'NONE', #18556, #13698, #12929, .T. ) ;
#14298 = ADVANCED_FACE ( 'NONE', ( #17604 ), #13111, .T. ) ;
#14299 = ORIENTED_EDGE ( 'NONE', *, *, #14926, .F. ) ;
#14300 = CARTESIAN_POINT ( 'NONE',  ( -4.477846259693480491, 50.66141209518846011, 54.55433879953098852 ) ) ;
#14301 = CARTESIAN_POINT ( 'NONE',  ( 4.454345183533989783, 39.79502090995749342, 90.27410581162071423 ) ) ;
#14302 = ORIENTED_EDGE ( 'NONE', *, *, #206, .F. ) ;
#14303 = CARTESIAN_POINT ( 'NONE',  ( 9.271561067608034890, 45.68041113525027441, 79.47125056423675460 ) ) ;
#14304 = CARTESIAN_POINT ( 'NONE',  ( -6.782631326057145138, 43.38225751353197523, 75.45433879953087342 ) ) ;
#14305 = CARTESIAN_POINT ( 'NONE',  ( 0.8043224091395101416, 52.95766084152177910, 78.82132898185037106 ) ) ;
#14306 = CARTESIAN_POINT ( 'NONE',  ( 4.155794158978344477, 39.80096085272940343, 95.60097222790500382 ) ) ;
#14307 = CONTEXT_DEPENDENT_SHAPE_REPRESENTATION ( #7353, #2249 ) ;
#14308 = CARTESIAN_POINT ( 'NONE',  ( -3.755902984582861759, 36.38179493852598512, 77.82155188814751057 ) ) ;
#14309 = VECTOR ( 'NONE', #11402, 1000.000000000000114 ) ;
#14310 = CARTESIAN_POINT ( 'NONE',  ( 31.07218010054375412, 45.56218137147968861, 70.80574467885102763 ) ) ;
#14311 = CARTESIAN_POINT ( 'NONE',  ( 5.396193866099816105, 50.74770293185853376, 75.97260389846793771 ) ) ;
#14312 = ORIENTED_EDGE ( 'NONE', *, *, #1298, .F. ) ;
#14313 = CARTESIAN_POINT ( 'NONE',  ( 2.120837336286425678, 52.95414753789260942, 78.20017459567505114 ) ) ;
#14314 = LINE ( 'NONE', #20683, #15781 ) ;
#14315 = VERTEX_POINT ( 'NONE', #20884 ) ;
#14316 = DIRECTION ( 'NONE',  ( 2.838338907332122006E-16, -1.000000000000000000, 0.000000000000000000 ) ) ;
#14317 = EDGE_CURVE ( 'NONE', #15999, #20602, #11132, .T. ) ;
#14318 = CARTESIAN_POINT ( 'NONE',  ( 5.683893922249901642, 37.03479970459495263, 77.75763958275959453 ) ) ;
#14319 = CARTESIAN_POINT ( 'NONE',  ( 8.913594855155908547, 41.50833375100289402, 79.54698768757486960 ) ) ;
#14320 = CARTESIAN_POINT ( 'NONE',  ( 1.964251312053308718, 36.08998497932209659, 72.45433879953085921 ) ) ;
#14321 = ORIENTED_EDGE ( 'NONE', *, *, #13920, .F. ) ;
#14322 = CARTESIAN_POINT ( 'NONE',  ( 5.675263920727823042, 51.29620106613522523, 77.96371040190514634 ) ) ;
#14323 = ORIENTED_EDGE ( 'NONE', *, *, #1038, .F. ) ;
#14324 = VECTOR ( 'NONE', #15183, 1000.000000000000114 ) ;
#14325 = CARTESIAN_POINT ( 'NONE',  ( -4.233737104609306634, 36.73475175465707565, 75.41196988111011024 ) ) ;
#14326 = CARTESIAN_POINT ( 'NONE',  ( -4.557243880370990041, 36.97371317826440418, 76.05537227506185616 ) ) ;
#14327 = EDGE_CURVE ( 'NONE', #3932, #10333, #5817, .T. ) ;
#14328 = CARTESIAN_POINT ( 'NONE',  ( -5.360233167866653048, 49.87514610275245275, 76.07559164877143587 ) ) ;
#14329 = VECTOR ( 'NONE', #17224, 1000.000000000000000 ) ;
#14330 = ORIENTED_EDGE ( 'NONE', *, *, #2970, .F. ) ;
#14331 = CARTESIAN_POINT ( 'NONE',  ( -4.147362675617721095, 37.44571156211047480, 76.85096240152589075 ) ) ;
#14332 =( BOUNDED_CURVE ( )  B_SPLINE_CURVE ( 2, ( #12375, #12160, #10474, #18850, #12270, #16938, #4262, #10788, #18639, #20640, #18536, #1092, #2364, #4054, #9182, #17254, #14156, #3950, #17361, #7251, #5650, #10582, #1194, #13747, #15672, #8868, #7579, #15354, #14062, #20217, #17052, #20546, #18752, #9072, #976 ),
 .UNSPECIFIED., .F., .F. ) 
 B_SPLINE_CURVE_WITH_KNOTS ( ( 3, 2, 2, 2, 2, 2, 2, 2, 2, 2, 2, 2, 2, 2, 2, 2, 2, 3 ),
 ( 0.3161083822038468494, 0.3396651204095990084, 0.3736316324505708497, 0.4075981444915426355, 0.4415646565325144768, 0.4755311685734863181, 0.5094976806144581039, 0.5434641926554300007, 0.5774307046964017864, 0.6113972167373735722, 0.6453637287783454690, 0.6793302408193173658, 0.7132967528602891516, 0.7472632649012609374, 0.7812297769422327232, 0.8151962889832046200, 0.8491628010241764057, 0.8809549974670297656 ),
 .UNSPECIFIED. ) 
 CURVE ( )  GEOMETRIC_REPRESENTATION_ITEM ( )  RATIONAL_B_SPLINE_CURVE ( ( 0.9676416783630596985, 0.9472082996756301387, 1.000000000000000000, 0.9238795325112867385, 1.000000000000000000, 0.9238795325112867385, 1.000000000000000000, 0.9238795325112867385, 1.000000000000000000, 0.9238795325112867385, 1.000000000000000000, 0.9238795325112867385, 1.000000000000000000, 0.9238795325112867385, 1.000000000000000000, 0.9238795325112867385, 1.000000000000000000, 0.9238795325112867385, 1.000000000000000000, 0.9238795325112867385, 1.000000000000000000, 0.9238795325112867385, 1.000000000000000000, 0.9238795325112867385, 1.000000000000000000, 0.9238795325112867385, 1.000000000000000000, 0.9238795325112867385, 1.000000000000000000, 0.9238795325112867385, 1.000000000000000000, 0.9238795325112867385, 1.000000000000000000, 0.9287522706834349107, 0.9908783657858857286 ) ) 
 REPRESENTATION_ITEM ( '' )  );
#14333 = PLANE ( 'NONE',  #2034 ) ;
#14334 = CARTESIAN_POINT ( 'NONE',  ( -1.419351766502866541, 49.49642391118513274, 91.00121379782397923 ) ) ;
#14335 = EDGE_CURVE ( 'NONE', #8009, #10690, #6277, .T. ) ;
#14336 = ADVANCED_FACE ( 'NONE', ( #16381 ), #3387, .F. ) ;
#14337 = VERTEX_POINT ( 'NONE', #19453 ) ;
#14338 = LINE ( 'NONE', #9874, #19577 ) ;
#14339 = CARTESIAN_POINT ( 'NONE',  ( -7.891196933625220566, 41.56260028800092954, 79.54845644658969661 ) ) ;
#14340 = DIRECTION ( 'NONE',  ( -0.3165065846431829311, -0.9485903129789527988, -2.188653791613874255E-16 ) ) ;
#14341 = CARTESIAN_POINT ( 'NONE',  ( 2.043125170982144745, 38.48583871533720213, 91.42996380123798872 ) ) ;
#14342 = B_SPLINE_CURVE_WITH_KNOTS ( 'NONE', 3,
 ( #19494, #20869, #1634, #19283, #4697, #11429, #16108, #20968, #19391, #17902, #3324, #11223, #1747, #8014 ),
 .UNSPECIFIED., .F., .F.,
 ( 4, 2, 2, 2, 2, 2, 4 ),
 ( 0.000000000000000000, 0.0004305053772964893247, 0.0006457580659447340141, 0.0008610107545929786494, 0.001076263443241223718, 0.001291516131889468896, 0.001722021509185946240 ),
 .UNSPECIFIED. ) ;
#14343 = CARTESIAN_POINT ( 'NONE',  ( -5.050952507338172914, 50.99561590888721696, 75.40305853716382956 ) ) ;
#14344 = VECTOR ( 'NONE', #2767, 1000.000000000000114 ) ;
#14345 = DIRECTION ( 'NONE',  ( 1.000000000000000000, -1.110223024625156417E-16, -1.111814006898795283E-16 ) ) ;
#14346 = CARTESIAN_POINT ( 'NONE',  ( -4.303670962001103106, 50.79176777958974753, 75.36022115247205022 ) ) ;
#14347 = VECTOR ( 'NONE', #3640, 1000.000000000000000 ) ;
#14348 = CARTESIAN_POINT ( 'NONE',  ( -0.6541186644085422719, 52.97764124372373118, 79.16576412035692556 ) ) ;
#14349 = DIRECTION ( 'NONE',  ( 0.7071067811865517916, 0.7071067811865433539, -0.000000000000000000 ) ) ;
#14350 = CARTESIAN_POINT ( 'NONE',  ( 0.5221537403065008576, 44.16218137147968292, 80.45433879953087342 ) ) ;
#14351 = DIRECTION ( 'NONE',  ( 1.000000000000000000, 3.620524460287505751E-17, 3.893792155548169402E-16 ) ) ;
#14352 = DIRECTION ( 'NONE',  ( -1.779391786395883536E-16, -5.922860397471806844E-17, 1.000000000000000000 ) ) ;
#14353 = EDGE_LOOP ( 'NONE', ( #15052, #19562, #9204, #12992, #5895 ) ) ;
#14354 = EDGE_CURVE ( 'NONE', #16139, #19569, #6678, .T. ) ;
#14355 = ORIENTED_EDGE ( 'NONE', *, *, #10703, .F. ) ;
#14356 = CIRCLE ( 'NONE', #19436, 6.200000000000000178 ) ;
#14357 = CARTESIAN_POINT ( 'NONE',  ( 9.350990972312333227, 42.81923766201297354, 78.59572304307680213 ) ) ;
#14358 = CARTESIAN_POINT ( 'NONE',  ( -4.056193511719762945, 50.96503781144581069, 76.08556810432578743 ) ) ;
#14359 = CARTESIAN_POINT ( 'NONE',  ( 6.924055141134583202, 50.37376929599953712, 78.48669174070734300 ) ) ;
#14360 = VECTOR ( 'NONE', #19864, 1000.000000000000227 ) ;
#14361 = LINE ( 'NONE', #2876, #17784 ) ;
#14362 = DIRECTION ( 'NONE',  ( 5.731934358295347564E-32, -3.469446951953617147E-16, -1.000000000000000000 ) ) ;
#14363 = CARTESIAN_POINT ( 'NONE',  ( 8.214799251806553571, 41.32260305165857517, 77.80727997600146750 ) ) ;
#14364 = LINE ( 'NONE', #12456, #15917 ) ;
#14365 = CARTESIAN_POINT ( 'NONE',  ( -4.504974378170068405, 37.87111029862571598, 79.54733240137164785 ) ) ;
#14366 = CIRCLE ( 'NONE', #13355, 6.200000000000000178 ) ;
#14367 = EDGE_CURVE ( 'NONE', #9681, #3298, #96, .T. ) ;
#14368 = CARTESIAN_POINT ( 'NONE',  ( 2.522153740306505743, 50.16218137147969713, 82.55433879953099563 ) ) ;
#14369 = DIRECTION ( 'NONE',  ( 1.779391786395883536E-16, 5.922860397471806844E-17, -1.000000000000000000 ) ) ;
#14370 = VERTEX_POINT ( 'NONE', #13082 ) ;
#14371 = DIRECTION ( 'NONE',  ( 0.3165065846431827645, 0.9485903129789529098, 0.000000000000000000 ) ) ;
#14372 = CARTESIAN_POINT ( 'NONE',  ( -3.943187491250720544, 40.73580453397070755, 90.64871380294496817 ) ) ;
#14373 = VERTEX_POINT ( 'NONE', #4974 ) ;
#14374 = CARTESIAN_POINT ( 'NONE',  ( -0.9236265496033003730, 52.97854115207936587, 76.40919915166844589 ) ) ;
#14375 = CARTESIAN_POINT ( 'NONE',  ( 8.398749874130045256, 41.92016587269467465, 78.13399373581940210 ) ) ;
#14376 = DIRECTION ( 'NONE',  ( -4.731737692062791983E-17, 0.7071067811865500152, 0.7071067811865451302 ) ) ;
#14377 = SURFACE_STYLE_FILL_AREA ( #20948 ) ;
#14378 = CARTESIAN_POINT ( 'NONE',  ( 3.725227782951431976, 48.32835457620019781, 92.45433879953095868 ) ) ;
#14379 = VERTEX_POINT ( 'NONE', #9903 ) ;
#14380 = CARTESIAN_POINT ( 'NONE',  ( -1.477846259693490705, 50.16218137147969713, 58.55433879953100984 ) ) ;
#14381 = VECTOR ( 'NONE', #7121, 1000.000000000000000 ) ;
#14382 = ORIENTED_EDGE ( 'NONE', *, *, #20294, .F. ) ;
#14383 = CARTESIAN_POINT ( 'NONE',  ( 6.575359255040893913, 44.22010074469034180, 75.45433879953087342 ) ) ;
#14384 = ADVANCED_FACE ( 'NONE', ( #295 ), #1811, .F. ) ;
#14385 = DIRECTION ( 'NONE',  ( -1.402518428993831183E-16, 1.000000000000000000, 0.000000000000000000 ) ) ;
#14386 = CARTESIAN_POINT ( 'NONE',  ( 0.5446115036918264263, 52.36219191590829070, 75.97284715574890868 ) ) ;
#14387 = DIRECTION ( 'NONE',  ( -1.110223024625156540E-16, -1.000000000000000000, -5.922860397471808077E-17 ) ) ;
#14388 = CARTESIAN_POINT ( 'NONE',  ( 28.43948732994508077, 36.35905713404685713, 76.90433879953101837 ) ) ;
#14389 = B_SPLINE_CURVE_WITH_KNOTS ( 'NONE', 3,
 ( #7428, #13923, #2755, #5943 ),
 .UNSPECIFIED., .F., .F.,
 ( 4, 4 ),
 ( 0.000000000000000000, 0.002523081261280060890 ),
 .UNSPECIFIED. ) ;
#14390 = ORIENTED_EDGE ( 'NONE', *, *, #5279, .F. ) ;
#14391 = LINE ( 'NONE', #9310, #6759 ) ;
#14392 = ADVANCED_FACE ( 'NONE', ( #13184 ), #10006, .F. ) ;
#14393 = ORIENTED_EDGE ( 'NONE', *, *, #10455, .F. ) ;
#14394 = AXIS2_PLACEMENT_3D ( 'NONE', #7092, #13594, #7205 ) ;
#14395 = CARTESIAN_POINT ( 'NONE',  ( -3.364214957493191438, 51.28112122432482778, 75.54713691134779197 ) ) ;
#14396 = EDGE_CURVE ( 'NONE', #4661, #16560, #18179, .T. ) ;
#14397 = CARTESIAN_POINT ( 'NONE',  ( -3.350035803220276609, 49.20851703305431357, 95.88308880123798872 ) ) ;
#14398 = CARTESIAN_POINT ( 'NONE',  ( 4.539819439306699955, 52.13490816606735478, 76.55090572632929025 ) ) ;
#14399 = EDGE_LOOP ( 'NONE', ( #14678, #12281, #8966, #13142 ) ) ;
#14400 = DIRECTION ( 'NONE',  ( 0.8043570849667693867, -0.5941461771851783702, 1.733862608106223493E-17 ) ) ;
#14401 = CARTESIAN_POINT ( 'NONE',  ( 3.983393151002395438, 36.72848634532710577, 72.45433879953087342 ) ) ;
#14402 = CARTESIAN_POINT ( 'NONE',  ( 6.212565296439490403, 37.41256891269643603, 78.35997004935869370 ) ) ;
#14403 = CARTESIAN_POINT ( 'NONE',  ( 5.740585635973908474, 51.24795054640212300, 75.97198585835440099 ) ) ;
#14404 = CARTESIAN_POINT ( 'NONE',  ( 0.5221537403065181771, 44.16218137147969003, 56.15433879953099705 ) ) ;
#14405 = ORIENTED_EDGE ( 'NONE', *, *, #10529, .T. ) ;
#14406 = CARTESIAN_POINT ( 'NONE',  ( -7.290527651941959952, 40.11224193202943411, 78.50801527011910252 ) ) ;
#14407 = CARTESIAN_POINT ( 'NONE',  ( 0.9390242073577395043, 52.35189112169444314, 76.77576052100340576 ) ) ;
#14408 = VERTEX_POINT ( 'NONE', #19980 ) ;
#14409 = CARTESIAN_POINT ( 'NONE',  ( 0.01393779443975506731, 49.47836700364563711, 95.05433879953096721 ) ) ;
#14410 = DIRECTION ( 'NONE',  ( -1.540237394707283727E-16, -1.793354297423763257E-16, 1.000000000000000000 ) ) ;
#14411 = CARTESIAN_POINT ( 'NONE',  ( -5.838255805151811195, 50.43303779728307745, 76.65235776097600251 ) ) ;
#14412 = CARTESIAN_POINT ( 'NONE',  ( 0.2541436421823710656, 38.02374091943176637, 92.95433879782399345 ) ) ;
#14413 = DIRECTION ( 'NONE',  ( -1.779391786395883536E-16, -5.922860397471806844E-17, 1.000000000000000000 ) ) ;
#14414 = DIRECTION ( 'NONE',  ( -3.211742425186504723E-16, 5.922860397471811774E-17, -1.000000000000000000 ) ) ;
#14415 = CARTESIAN_POINT ( 'NONE',  ( 5.379940827581938478, 50.75970839669935941, 75.97198585835440099 ) ) ;
#14416 = ORIENTED_EDGE ( 'NONE', *, *, #15463, .F. ) ;
#14417 = CARTESIAN_POINT ( 'NONE',  ( 31.07218010054375412, 45.56218137147968861, 70.80574467885102763 ) ) ;
#14418 = CARTESIAN_POINT ( 'NONE',  ( 9.176231272041631470, 45.98187388689780164, 75.44992703482499508 ) ) ;
#14419 = ORIENTED_EDGE ( 'NONE', *, *, #18579, .F. ) ;
#14420 = CARTESIAN_POINT ( 'NONE',  ( 0.5221537403065085181, 49.16218137147969003, 93.04136871766880290 ) ) ;
#14421 = EDGE_CURVE ( 'NONE', #3162, #8610, #19130, .T. ) ;
#14422 = CARTESIAN_POINT ( 'NONE',  ( -0.9276151719557895747, 52.23300467605542252, 76.37477783580860091 ) ) ;
#14423 = CARTESIAN_POINT ( 'NONE',  ( 9.353718648869055130, 42.82741268169404947, 78.44945682776121032 ) ) ;
#14424 = CARTESIAN_POINT ( 'NONE',  ( 8.638826686988997139, 40.68483612003910110, 79.45050910333212357 ) ) ;
#14425 = VERTEX_POINT ( 'NONE', #18191 ) ;
#14426 = CARTESIAN_POINT ( 'NONE',  ( 5.568489401881125289, 48.03437091500647682, 94.32058880123798872 ) ) ;
#14427 = ORIENTED_EDGE ( 'NONE', *, *, #11991, .T. ) ;
#14428 = CARTESIAN_POINT ( 'NONE',  ( -4.074436747594614161, 36.61708299794012333, 75.46341390175899733 ) ) ;
#14429 = CARTESIAN_POINT ( 'NONE',  ( -4.532046673723622021, 36.95510101671938941, 76.17409373158149322 ) ) ;
#14430 = CARTESIAN_POINT ( 'NONE',  ( -2.904223097202481174, 48.62752260303690122, 95.02371379953099506 ) ) ;
#14431 = ORIENTED_EDGE ( 'NONE', *, *, #12758, .T. ) ;
#14432 = FACE_OUTER_BOUND ( 'NONE', #3957, .T. ) ;
#14433 = CARTESIAN_POINT ( 'NONE',  ( -7.261744020088604756, 41.57725440279298823, 79.54647244615752300 ) ) ;
#14434 = CARTESIAN_POINT ( 'NONE',  ( 2.232254456934871900, 39.46371826755015633, 92.48558879953097289 ) ) ;
#14435 = ORIENTED_EDGE ( 'NONE', *, *, #9229, .F. ) ;
#14436 = CARTESIAN_POINT ( 'NONE',  ( 2.527576913102087985, 36.82540565608436367, 75.45433879953087342 ) ) ;
#14437 = CARTESIAN_POINT ( 'NONE',  ( -6.374721436948748376, 46.24015083227975964, 79.45433879953087342 ) ) ;
#14438 = CARTESIAN_POINT ( 'NONE',  ( 10.77494014480653561, 42.96218137147968008, 74.20433879953100131 ) ) ;
#14439 = CARTESIAN_POINT ( 'NONE',  ( -5.784195910403845176, 44.99242805365518194, 92.28933880123798872 ) ) ;
#14440 = EDGE_CURVE ( 'NONE', #57, #18234, #10448, .T. ) ;
#14441 =( NAMED_UNIT ( * ) PLANE_ANGLE_UNIT ( ) SI_UNIT ( $, .RADIAN. ) );
#14442 = EDGE_CURVE ( 'NONE', #19814, #13351, #11817, .T. ) ;
#14443 = CARTESIAN_POINT ( 'NONE',  ( -5.825614074793430852, 50.44207111495388318, 76.36675183022860836 ) ) ;
#14444 = CARTESIAN_POINT ( 'NONE',  ( 27.03948732994508930, 45.16218137147969003, 76.90433879953101837 ) ) ;
#14445 = CARTESIAN_POINT ( 'NONE',  ( 8.833159395675938441, 41.26726357621102181, 77.50846324053436831 ) ) ;
#14446 = EDGE_CURVE ( 'NONE', #7497, #12733, #14366, .T. ) ;
#14447 = CARTESIAN_POINT ( 'NONE',  ( 26.27839330960314257, 24.25869832947912030, 85.06527890720686003 ) ) ;
#14448 = EDGE_CURVE ( 'NONE', #3841, #4878, #3610, .T. ) ;
#14449 = CARTESIAN_POINT ( 'NONE',  ( -0.9426531034333153203, 52.21747571285902012, 78.07640427701528552 ) ) ;
#14450 = ORIENTED_EDGE ( 'NONE', *, *, #18602, .T. ) ;
#14451 = LINE ( 'NONE', #20917, #20413 ) ;
#14452 = CARTESIAN_POINT ( 'NONE',  ( 8.640860003252242905, 43.05534814838419777, 76.37534566197098229 ) ) ;
#14453 = CARTESIAN_POINT ( 'NONE',  ( 0.7863323750428190539, 52.35808013066139210, 76.03473341409473107 ) ) ;
#14454 = CARTESIAN_POINT ( 'NONE',  ( 2.122153740306512937, 47.82824192744436687, 53.55433879953100273 ) ) ;
#14455 = EDGE_CURVE ( 'NONE', #3770, #15492, #7224, .T. ) ;
#14456 =( BOUNDED_SURFACE ( )  B_SPLINE_SURFACE ( 1, 2, ( 
 ( #1556, #12079, #3662, #16452, #11667, #13668, #16861, #13455, #18241, #8359, #3563, #572, #11979, #1871, #18559, #8572, #10283, #14944, #18455, #11766, #2180, #13555, #2076, #14840, #7168, #3870, #19927, #10392, #15059, #19829, #6853, #9970, #689, #10173, #7055, #5250, #8463, #16655, #259, #6748, #20033, #3764, #13253, #15160, #18144, #19729, #15269, #10068, #472, #6950, #5147, #5355, #16550, #20143, #2280, #11868, #8779, #18345, #16760, #13359, #1970, #5575, #8680, #5465, #366, #10498, #16962, #3972, #2392, #8893, #15381, #15003, #8830, #11814, #8518, #8939, #18290, #3821, #13502 ),
 ( #13720, #3922, #10446, #5729, #626, #10341, #16813, #20194, #15327, #5626, #19880, #12133, #2230, #13821, #8725, #18401, #422, #2447, #7330, #15214, #16908, #16708, #20087, #7107, #737, #3708, #12236, #6907, #519, #3608, #7220, #16599, #10230, #18610, #5524, #20299, #10117, #2335, #13408, #4024, #13610, #10550, #12035, #18509, #17017, #2131, #2020, #15428, #5404, #7001, #15113, #8633, #19978, #844, #11925, #5300, #4553, #12347, #9155, #7655, #18828, #14135, #14236, #10866, #17337, #9469, #6046, #11070, #1063, #2864, #17539, #19142, #15533, #12445, #20617, #10761, #2962, #4235, #4133 ) ),
 .UNSPECIFIED., .F., .F., .F. ) 
 B_SPLINE_SURFACE_WITH_KNOTS ( ( 2, 2 ),
 ( 3, 2, 2, 2, 2, 2, 2, 2, 2, 2, 2, 2, 2, 2, 2, 2, 2, 2, 2, 2, 2, 2, 2, 2, 2, 2, 2, 2, 2, 2, 2, 2, 2, 2, 2, 2, 2, 2, 2, 3 ),
 ( 0.000000000000000000, 1.000000000000000000 ),
 ( 0.000000000000000000, 0.02500000000000000139, 0.05000000000000000278, 0.07499999999999999722, 0.1000000000000000056, 0.1250000000000000000, 0.1499999999999999944, 0.1749999999999999889, 0.2000000000000000111, 0.2250000000000000056, 0.2500000000000000000, 0.2750000000000000222, 0.2999999999999999889, 0.3250000000000000111, 0.3499999999999999778, 0.3750000000000000000, 0.4000000000000000222, 0.4249999999999999889, 0.4500000000000000111, 0.4749999999999999778, 0.5000000000000000000, 0.5250000000000000222, 0.5500000000000000444, 0.5749999999999999556, 0.5999999999999999778, 0.6250000000000000000, 0.6500000000000000222, 0.6750000000000000444, 0.6999999999999999556, 0.7249999999999999778, 0.7500000000000000000, 0.7750000000000000222, 0.8000000000000000444, 0.8249999999999999556, 0.8499999999999999778, 0.8750000000000000000, 0.9000000000000000222, 0.9250000000000000444, 0.9499999999999999556, 0.9600310108036838042 ),
 .UNSPECIFIED. ) 
 GEOMETRIC_REPRESENTATION_ITEM ( )  RATIONAL_B_SPLINE_SURFACE ( (
 ( 1.000000000000000000, 0.9238795325112867385, 1.000000000000000000, 0.9238795325112867385, 1.000000000000000000, 0.9238795325112867385, 1.000000000000000000, 0.9238795325112867385, 1.000000000000000000, 0.9238795325112867385, 1.000000000000000000, 0.9238795325112867385, 1.000000000000000000, 0.9238795325112867385, 1.000000000000000000, 0.9238795325112867385, 1.000000000000000000, 0.9238795325112867385, 1.000000000000000000, 0.9238795325112867385, 1.000000000000000000, 0.9238795325112867385, 1.000000000000000000, 0.9238795325112867385, 1.000000000000000000, 0.9238795325112867385, 1.000000000000000000, 0.9238795325112867385, 1.000000000000000000, 0.9238795325112867385, 1.000000000000000000, 0.9238795325112867385, 1.000000000000000000, 0.9238795325112867385, 1.000000000000000000, 0.9238795325112867385, 1.000000000000000000, 0.9238795325112867385, 1.000000000000000000, 0.9238795325112867385, 1.000000000000000000, 0.9238795325112867385, 1.000000000000000000, 0.9238795325112867385, 1.000000000000000000, 0.9238795325112867385, 1.000000000000000000, 0.9238795325112867385, 1.000000000000000000, 0.9238795325112867385, 1.000000000000000000, 0.9238795325112867385, 1.000000000000000000, 0.9238795325112867385, 1.000000000000000000, 0.9238795325112867385, 1.000000000000000000, 0.9238795325112867385, 1.000000000000000000, 0.9238795325112867385, 1.000000000000000000, 0.9238795325112867385, 1.000000000000000000, 0.9238795325112867385, 1.000000000000000000, 0.9238795325112867385, 1.000000000000000000, 0.9238795325112867385, 1.000000000000000000, 0.9238795325112867385, 1.000000000000000000, 0.9238795325112867385, 1.000000000000000000, 0.9238795325112867385, 1.000000000000000000, 0.9238795325112867385, 1.000000000000000000, 0.9694573907295700455, 0.9634246409442903669),
 ( 1.000000000000000000, 0.9238795325112867385, 1.000000000000000000, 0.9238795325112867385, 1.000000000000000000, 0.9238795325112867385, 1.000000000000000000, 0.9238795325112867385, 1.000000000000000000, 0.9238795325112867385, 1.000000000000000000, 0.9238795325112867385, 1.000000000000000000, 0.9238795325112867385, 1.000000000000000000, 0.9238795325112867385, 1.000000000000000000, 0.9238795325112867385, 1.000000000000000000, 0.9238795325112867385, 1.000000000000000000, 0.9238795325112867385, 1.000000000000000000, 0.9238795325112867385, 1.000000000000000000, 0.9238795325112867385, 1.000000000000000000, 0.9238795325112867385, 1.000000000000000000, 0.9238795325112867385, 1.000000000000000000, 0.9238795325112867385, 1.000000000000000000, 0.9238795325112867385, 1.000000000000000000, 0.9238795325112867385, 1.000000000000000000, 0.9238795325112867385, 1.000000000000000000, 0.9238795325112867385, 1.000000000000000000, 0.9238795325112867385, 1.000000000000000000, 0.9238795325112867385, 1.000000000000000000, 0.9238795325112867385, 1.000000000000000000, 0.9238795325112867385, 1.000000000000000000, 0.9238795325112867385, 1.000000000000000000, 0.9238795325112867385, 1.000000000000000000, 0.9238795325112867385, 1.000000000000000000, 0.9238795325112867385, 1.000000000000000000, 0.9238795325112867385, 1.000000000000000000, 0.9238795325112867385, 1.000000000000000000, 0.9238795325112867385, 1.000000000000000000, 0.9238795325112867385, 1.000000000000000000, 0.9238795325112867385, 1.000000000000000000, 0.9238795325112867385, 1.000000000000000000, 0.9238795325112867385, 1.000000000000000000, 0.9238795325112867385, 1.000000000000000000, 0.9238795325112867385, 1.000000000000000000, 0.9238795325112867385, 1.000000000000000000, 0.9694573907295700455, 0.9634246409442903669) ) ) 
 REPRESENTATION_ITEM ( '' )  SURFACE ( )  );
#14457 = EDGE_LOOP ( 'NONE', ( #20875, #5079, #13791, #8326 ) ) ;
#14458 = ORIENTED_EDGE ( 'NONE', *, *, #15377, .T. ) ;
#14459 = CARTESIAN_POINT ( 'NONE',  ( 9.353817388681445522, 42.82770861117572281, 76.74257409364852833 ) ) ;
#14460 = CARTESIAN_POINT ( 'NONE',  ( 8.300594306733913186, 41.56682737740558764, 77.52492703482499792 ) ) ;
#14461 = CARTESIAN_POINT ( 'NONE',  ( 5.127341568105101999, 37.37742690587217709, 77.69977153848151374 ) ) ;
#14462 = CARTESIAN_POINT ( 'NONE',  ( 4.831344325983889298, 51.13914440238564652, 79.48349463613192256 ) ) ;
#14463 = CARTESIAN_POINT ( 'NONE',  ( -3.154801521863567881, 47.83913663364971569, 93.80036078214054385 ) ) ;
#14464 = FACE_OUTER_BOUND ( 'NONE', #2620, .T. ) ;
#14465 = CARTESIAN_POINT ( 'NONE',  ( 6.462739881952892063, 49.81458902753052342, 78.15691020095597707 ) ) ;
#14466 = CARTESIAN_POINT ( 'NONE',  ( -1.077846259693493458, 50.16218137147969713, 61.55433879953100273 ) ) ;
#14467 = CARTESIAN_POINT ( 'NONE',  ( 9.315603341877332966, 42.71317868864986877, 77.73063109826868811 ) ) ;
#14468 = DIRECTION ( 'NONE',  ( 0.000000000000000000, -1.000000000000000000, 0.000000000000000000 ) ) ;
#14469 = CARTESIAN_POINT ( 'NONE',  ( 5.309312511458522899, 50.81985754494123597, 75.97849039075508415 ) ) ;
#14470 = ADVANCED_FACE ( 'NONE', ( #13309 ), #10120, .T. ) ;
#14471 = CARTESIAN_POINT ( 'NONE',  ( 8.790412360755954779, 41.13914800073450095, 78.76104738055306598 ) ) ;
#14472 = CARTESIAN_POINT ( 'NONE',  ( 0.8261150126163424590, 52.35656485298985530, 78.75698059774664728 ) ) ;
#14473 = CARTESIAN_POINT ( 'NONE',  ( 0.5855440626654981884, 51.36190535648659505, 75.36022115247205022 ) ) ;
#14474 = VERTEX_POINT ( 'NONE', #12037 ) ;
#14475 = CARTESIAN_POINT ( 'NONE',  ( -6.427915807670530945, 42.26053564693651055, 78.50654468188380974 ) ) ;
#14476 = CARTESIAN_POINT ( 'NONE',  ( 9.080605399405701661, 42.00887494707089331, 78.12791555553386047 ) ) ;
#14477 = ORIENTED_EDGE ( 'NONE', *, *, #15206, .F. ) ;
#14478 = CARTESIAN_POINT ( 'NONE',  ( 6.880792506138228681, 37.89005961138749967, 76.49840989696882332 ) ) ;
#14479 = CARTESIAN_POINT ( 'NONE',  ( 0.5221537403064990812, 44.16218137147969003, 95.05433879953096721 ) ) ;
#14480 = DIRECTION ( 'NONE',  ( -1.540237394707284220E-16, -1.793354297423764243E-16, 1.000000000000000000 ) ) ;
#14481 = DIRECTION ( 'NONE',  ( -0.5813877811926999595, 0.8136266022444381685, -1.516940570386243703E-15 ) ) ;
#14482 = LINE ( 'NONE', #20748, #17412 ) ;
#14483 = VERTEX_POINT ( 'NONE', #20196 ) ;
#14484 = DIRECTION ( 'NONE',  ( -1.110223024625156540E-16, -1.000000000000000000, -5.922860397471808077E-17 ) ) ;
#14485 = AXIS2_PLACEMENT_3D ( 'NONE', #10895, #12474, #7683 ) ;
#14486 = ORIENTED_EDGE ( 'NONE', *, *, #17656, .F. ) ;
#14487 = CARTESIAN_POINT ( 'NONE',  ( -0.3080929418689875576, 37.85583172076933778, 94.94558880123797451 ) ) ;
#14488 = CARTESIAN_POINT ( 'NONE',  ( -4.567115856812060670, 47.10047254335474065, 93.30496380123798872 ) ) ;
#14489 = LINE ( 'NONE', #6496, #14574 ) ;
#14490 = CARTESIAN_POINT ( 'NONE',  ( 5.848951923618479931, 37.15274410921379911, 76.58742703482498371 ) ) ;
#14491 = CARTESIAN_POINT ( 'NONE',  ( -5.933958468462559921, 37.99063678704128932, 76.24300064276494027 ) ) ;
#14492 = EDGE_LOOP ( 'NONE', ( #4481, #2372, #8262, #6958 ) ) ;
#14493 = PLANE ( 'NONE',  #2027 ) ;
#14494 = ORIENTED_EDGE ( 'NONE', *, *, #17955, .T. ) ;
#14495 = AXIS2_PLACEMENT_3D ( 'NONE', #15541, #20308, #636 ) ;
#14496 = DIRECTION ( 'NONE',  ( 0.5813877811927011807, -0.8136266022444372803, -5.636455622144619183E-17 ) ) ;
#14497 = CARTESIAN_POINT ( 'NONE',  ( 5.611423337425062385, 41.22389019960463230, 90.33621380123798872 ) ) ;
#14498 = CARTESIAN_POINT ( 'NONE',  ( 5.389492195292208798, 36.82443100924615464, 78.79551527011911105 ) ) ;
#14499 = VERTEX_POINT ( 'NONE', #8520 ) ;
#14500 = EDGE_CURVE ( 'NONE', #445, #19138, #5303, .T. ) ;
#14501 = DIRECTION ( 'NONE',  ( -1.402518428993831183E-16, 1.000000000000000000, -3.469446951953617640E-16 ) ) ;
#14502 = CARTESIAN_POINT ( 'NONE',  ( 5.434012744193106315, 45.09686908721048582, 92.45433879953098710 ) ) ;
#14503 = CARTESIAN_POINT ( 'NONE',  ( 5.933960187751527116, 51.10511255460609448, 76.21496574784163158 ) ) ;
#14504 = CARTESIAN_POINT ( 'NONE',  ( -0.08445379298374396104, 38.30427143568992676, 95.05433879953095300 ) ) ;
#14505 = CARTESIAN_POINT ( 'NONE',  ( 0.5221537403065015237, 44.16218137147968292, 75.45433879953088763 ) ) ;
#14506 = VERTEX_POINT ( 'NONE', #14887 ) ;
#14507 = CARTESIAN_POINT ( 'NONE',  ( -4.235929252861276417, 41.08920907837907777, 92.55433879953100984 ) ) ;
#14508 = DIRECTION ( 'NONE',  ( -1.193617070626243484E-16, -1.000000000000000000, -0.000000000000000000 ) ) ;
#14509 = EDGE_LOOP ( 'NONE', ( #20770, #12713, #11424, #12909, #2627 ) ) ;
#14510 = CARTESIAN_POINT ( 'NONE',  ( 0.6695212169850585093, 49.45709967392639328, 95.05433879953099563 ) ) ;
#14511 = CARTESIAN_POINT ( 'NONE',  ( 0.5221537403065188432, 44.16218137147969003, 54.55433879953099563 ) ) ;
#14512 = CARTESIAN_POINT ( 'NONE',  ( 2.538045550429134600, 49.87014351810298507, 72.45433879953087342 ) ) ;
#14513 = B_SPLINE_CURVE_WITH_KNOTS ( 'NONE', 3,
 ( #1104, #7791, #15575, #14275, #2800, #20754, #990, #20456, #4275, #19269, #9506, #10800 ),
 .UNSPECIFIED., .F., .F.,
 ( 4, 2, 2, 2, 2, 4 ),
 ( 0.000000000000000000, 0.0001995372338163474250, 0.0003990744676326948501, 0.0007981489352653508857, 0.001197223402898007138, 0.001596297870530663174 ),
 .UNSPECIFIED. ) ;
#14514 = CARTESIAN_POINT ( 'NONE',  ( 30.92220646078100188, 42.96218137147968008, 57.80715055817105252 ) ) ;
#14515 = CARTESIAN_POINT ( 'NONE',  ( -1.187946976321872405, 48.86064447540922373, 94.04808879611699979 ) ) ;
#14516 = VECTOR ( 'NONE', #11156, 1000.000000000000000 ) ;
#14517 = CONTEXT_DEPENDENT_SHAPE_REPRESENTATION ( #10242, #17862 ) ;
#14518 = CARTESIAN_POINT ( 'NONE',  ( -5.616286711741429905, 44.43019146960381960, 92.48558879782397923 ) ) ;
#14519 = DIRECTION ( 'NONE',  ( -1.540237394707284220E-16, -1.793354297423764243E-16, 1.000000000000000000 ) ) ;
#14520 = CARTESIAN_POINT ( 'NONE',  ( -3.053082554203018439, 36.78748274492485137, 76.62933879953087057 ) ) ;
#14521 = ORIENTED_EDGE ( 'NONE', *, *, #8084, .F. ) ;
#14522 = CARTESIAN_POINT ( 'NONE',  ( -1.202011496911928434, 49.96493122755408223, 75.45433879953087342 ) ) ;
#14523 = CARTESIAN_POINT ( 'NONE',  ( -3.518392077816012709, 37.12037020444837765, 77.68963291717793140 ) ) ;
#14524 = CONICAL_SURFACE ( 'NONE', #8424, 6.200000000000020606, 1.047197551196600518 ) ;
#14525 = ORIENTED_EDGE ( 'NONE', *, *, #6361, .T. ) ;
#14526 = DIRECTION ( 'NONE',  ( -0.3165065846431827645, -0.9485903129789529098, 0.000000000000000000 ) ) ;
#14527 = ADVANCED_FACE ( 'NONE', ( #15217 ), #425, .T. ) ;
#14528 = CARTESIAN_POINT ( 'NONE',  ( 4.135038682601217097, 47.90320695352507130, 92.55433879953098142 ) ) ;
#14529 = DIRECTION ( 'NONE',  ( 0.07958035169224103589, -0.2516580640468327190, -0.9645388465089104191 ) ) ;
#14530 = ORIENTED_EDGE ( 'NONE', *, *, #1283, .F. ) ;
#14531 = CARTESIAN_POINT ( 'NONE',  ( 5.599756831756513620, 51.35197511114724733, 78.21422674182478829 ) ) ;
#14532 = ORIENTED_EDGE ( 'NONE', *, *, #9631, .F. ) ;
#14533 = VECTOR ( 'NONE', #13800, 1000.000000000000000 ) ;
#14534 = EDGE_CURVE ( 'NONE', #2768, #7833, #16815, .T. ) ;
#14535 = PLANE ( 'NONE',  #5711 ) ;
#14536 = CARTESIAN_POINT ( 'NONE',  ( -4.177068838871750955, 37.44752913149660856, 76.12832907849806929 ) ) ;
#14537 = CARTESIAN_POINT ( 'NONE',  ( 3.122153740306552905, 48.66551347115873227, 96.03933879953099506 ) ) ;
#14538 = ORIENTED_EDGE ( 'NONE', *, *, #11608, .T. ) ;
#14539 = DIRECTION ( 'NONE',  ( 1.540237394707284220E-16, 1.793354297423764243E-16, -1.000000000000000000 ) ) ;
#14540 = CARTESIAN_POINT ( 'NONE',  ( -6.830989029115968947, 40.53234436544566677, 79.14164642658485604 ) ) ;
#14541 = CARTESIAN_POINT ( 'NONE',  ( 0.2860873169776710356, 38.75537135769874197, 92.40746379953097289 ) ) ;
#14542 = ORIENTED_EDGE ( 'NONE', *, *, #19825, .T. ) ;
#14543 = CARTESIAN_POINT ( 'NONE',  ( -4.788785806866687089, 51.18295063450860738, 76.15325518536063498 ) ) ;
#14544 = CARTESIAN_POINT ( 'NONE',  ( -0.4699484075729998822, 52.36218137147968577, 83.03825919817350609 ) ) ;
#14545 = DIRECTION ( 'NONE',  ( -0.9485903129789527988, 0.3165065846431829311, -8.934458285744989980E-17 ) ) ;
#14546 = VECTOR ( 'NONE', #9505, 1000.000000000000000 ) ;
#14547 =( NAMED_UNIT ( * ) PLANE_ANGLE_UNIT ( ) SI_UNIT ( $, .RADIAN. ) );
#14548 = CARTESIAN_POINT ( 'NONE',  ( -3.350035803220276609, 49.20851703305431357, 93.22683880123798872 ) ) ;
#14549 = EDGE_CURVE ( 'NONE', #15405, #7189, #13341, .T. ) ;
#14550 = CARTESIAN_POINT ( 'NONE',  ( 6.100231826182790584, 38.15139326043413348, 78.27625046823177968 ) ) ;
#14551 = EDGE_CURVE ( 'NONE', #14408, #9268, #18439, .T. ) ;
#14552 = CARTESIAN_POINT ( 'NONE',  ( 8.791848479292760032, 41.14345213909496835, 77.32915800260404637 ) ) ;
#14553 = CARTESIAN_POINT ( 'NONE',  ( 5.427780505986065762, 36.85179043424346190, 77.43080938776617472 ) ) ;
#14554 = CARTESIAN_POINT ( 'NONE',  ( -0.9162890130466297967, 52.97970855327192652, 78.60293901857092180 ) ) ;
#14555 = ORIENTED_EDGE ( 'NONE', *, *, #6448, .T. ) ;
#14556 = DIRECTION ( 'NONE',  ( -0.3165065846431775465, -0.9485903129789546862, 0.000000000000000000 ) ) ;
#14557 = CARTESIAN_POINT ( 'NONE',  ( 8.607671302521914924, 42.95587950684349465, 75.91044101036179370 ) ) ;
#14558 = ADVANCED_FACE ( 'NONE', ( #11928 ), #19883, .T. ) ;
#14559 = CARTESIAN_POINT ( 'NONE',  ( 8.400787919062072007, 39.97141883166423781, 78.77723610448765612 ) ) ;
#14560 = ADVANCED_FACE ( 'NONE', ( #522 ), #6819, .F. ) ;
#14561 = EDGE_CURVE ( 'NONE', #15567, #1015, #4135, .T. ) ;
#14562 = AXIS2_PLACEMENT_3D ( 'NONE', #4367, #15562, #10891 ) ;
#14563 = VERTEX_POINT ( 'NONE', #10666 ) ;
#14564 = ORIENTED_EDGE ( 'NONE', *, *, #3974, .F. ) ;
#14565 = CARTESIAN_POINT ( 'NONE',  ( 9.240682951717872129, 42.48863752648103542, 75.64289537645213102 ) ) ;
#14566 = ADVANCED_FACE ( 'NONE', ( #846 ), #10069, .F. ) ;
#14567 = CARTESIAN_POINT ( 'NONE',  ( -4.895465483855352851, 37.22354385236106111, 78.55727908454632313 ) ) ;
#14568 = CARTESIAN_POINT ( 'NONE',  ( 4.143017335158133641, 51.51944627275094746, 78.46169174070733732 ) ) ;
#14569 = LINE ( 'NONE', #6363, #19477 ) ;
#14570 = CARTESIAN_POINT ( 'NONE',  ( -1.117719678584870424, 36.12782917792895176, 72.45433879953085921 ) ) ;
#14571 = DIRECTION ( 'NONE',  ( -1.540237394707284220E-16, -1.793354297423764243E-16, 1.000000000000000000 ) ) ;
#14572 = CARTESIAN_POINT ( 'NONE',  ( 6.949446517235058352, 50.35501370930113296, 76.97234655072247733 ) ) ;
#14573 = CARTESIAN_POINT ( 'NONE',  ( 27.03948732994508930, 45.16218137147969003, 77.50433879953099847 ) ) ;
#14574 = VECTOR ( 'NONE', #21, 1000.000000000000000 ) ;
#14575 = ORIENTED_EDGE ( 'NONE', *, *, #19794, .T. ) ;
#14576 = CARTESIAN_POINT ( 'NONE',  ( 8.797946357469051293, 41.16172786683149099, 78.83414475571305502 ) ) ;
#14577 = DIRECTION ( 'NONE',  ( -1.084202172485505420E-16, -1.000000000000000000, 0.000000000000000000 ) ) ;
#14578 = DIRECTION ( 'NONE',  ( 0.007885122365275663500, 0.9999689119394085113, 1.805443505845543142E-16 ) ) ;
#14579 = CARTESIAN_POINT ( 'NONE',  ( 2.436687528221638033, 49.84925249003585179, 85.23980501161587142 ) ) ;
#14580 = EDGE_CURVE ( 'NONE', #1661, #11174, #3576, .T. ) ;
#14581 = CARTESIAN_POINT ( 'NONE',  ( 9.277577006266444215, 42.59921134847828483, 77.86785210695053649 ) ) ;
#14582 = ORIENTED_EDGE ( 'NONE', *, *, #17560, .T. ) ;
#14583 = VECTOR ( 'NONE', #20688, 1000.000000000000114 ) ;
#14584 = CARTESIAN_POINT ( 'NONE',  ( 0.1922742723289393996, 52.96974186399811657, 75.38460717221940399 ) ) ;
#14585 = CARTESIAN_POINT ( 'NONE',  ( 4.676321589340446394, 52.03407952647943091, 79.02133806855546538 ) ) ;
#14586 = CARTESIAN_POINT ( 'NONE',  ( 5.076572431691917409, 37.34329067111212197, 77.43080938776617472 ) ) ;
#14587 = CARTESIAN_POINT ( 'NONE',  ( 4.611431799778751284, 51.27033221398914975, 75.50754157125952304 ) ) ;
#14588 = ADVANCED_FACE ( 'NONE', ( #19419 ), #14634, .F. ) ;
#14589 = CARTESIAN_POINT ( 'NONE',  ( -2.627048034785010699, 48.88511640015991588, 92.45433879952862810 ) ) ;
#14590 = EDGE_LOOP ( 'NONE', ( #19445, #17309, #3590, #11647 ) ) ;
#14591 = CARTESIAN_POINT ( 'NONE',  ( -4.578222290571132724, 51.33341161403104280, 78.93596775356181183 ) ) ;
#14592 = EDGE_CURVE ( 'NONE', #9005, #2886, #1663, .T. ) ;
#14593 = ORIENTED_EDGE ( 'NONE', *, *, #6995, .F. ) ;
#14594 = CARTESIAN_POINT ( 'NONE',  ( -2.904223097202481174, 48.62752260303690122, 95.33621380294498238 ) ) ;
#14595 = AXIS2_PLACEMENT_3D ( 'NONE', #4087, #8900, #5909 ) ;
#14596 = CARTESIAN_POINT ( 'NONE',  ( 1.173218185867612506, 52.94769249949187895, 76.77301385304936332 ) ) ;
#14597 = CARTESIAN_POINT ( 'NONE',  ( 0.5221537403065091842, 44.16218137147969713, 58.55433879953100984 ) ) ;
#14598 = AXIS2_PLACEMENT_3D ( 'NONE', #11381, #17851, #9781 ) ;
#14599 = DIRECTION ( 'NONE',  ( 1.000000000000000000, 0.000000000000000000, 0.000000000000000000 ) ) ;
#14600 = EDGE_LOOP ( 'NONE', ( #5669, #7214, #7275, #17749, #4778, #16660, #17107 ) ) ;
#14601 = CARTESIAN_POINT ( 'NONE',  ( 5.241302188025125375, 50.86813933424380707, 77.20515338154341123 ) ) ;
#14602 = ORIENTED_EDGE ( 'NONE', *, *, #3647, .F. ) ;
#14603 = VECTOR ( 'NONE', #19531, 1000.000000000000000 ) ;
#14604 = LINE ( 'NONE', #9314, #9529 ) ;
#14605 = CARTESIAN_POINT ( 'NONE',  ( 1.352400422481993658, 50.46853102219002096, 90.72683880123797451 ) ) ;
#14606 = CARTESIAN_POINT ( 'NONE',  ( -5.154188915835984375, 42.64120994080404614, 95.96121380123798872 ) ) ;
#14607 = VERTEX_POINT ( 'NONE', #13050 ) ;
#14608 = CARTESIAN_POINT ( 'NONE',  ( -5.397178805542148794, 49.82826827278250903, 78.41225960292398156 ) ) ;
#14609 = DIRECTION ( 'NONE',  ( -1.000000000000000000, -1.402518428993831676E-16, -1.196361017915039239E-16 ) ) ;
#14610 = CARTESIAN_POINT ( 'NONE',  ( 5.787239255393352266, 51.21348939705941206, 75.97375991483075097 ) ) ;
#14611 = CARTESIAN_POINT ( 'NONE',  ( 0.5221537403065014127, 44.16218137147968292, 76.48963291717792856 ) ) ;
#14612 = DIRECTION ( 'NONE',  ( 0.007885122365275663500, 0.9999689119394085113, 1.805443505845543142E-16 ) ) ;
#14613 = VERTEX_POINT ( 'NONE', #16553 ) ;
#14614 = AXIS2_PLACEMENT_3D ( 'NONE', #5915, #18573, #10298 ) ;
#14615 = DIRECTION ( 'NONE',  ( 0.9480563259966798828, 0.3181025035074024343, 2.030702297275143506E-16 ) ) ;
#14616 = VECTOR ( 'NONE', #5672, 1000.000000000000114 ) ;
#14617 = CARTESIAN_POINT ( 'NONE',  ( 0.5264284712812515865, 52.36237607488513390, 76.89393222956012153 ) ) ;
#14618 = ORIENTED_EDGE ( 'NONE', *, *, #14981, .F. ) ;
#14619 = FACE_BOUND ( 'NONE', #6769, .T. ) ;
#14620 = CARTESIAN_POINT ( 'NONE',  ( 0.5221537403065010796, 44.16218137147969003, 54.55433879953099563 ) ) ;
#14621 = CARTESIAN_POINT ( 'NONE',  ( -4.264291154750528889, 50.63795972765758791, 75.36124333316173818 ) ) ;
#14622 = CARTESIAN_POINT ( 'NONE',  ( 4.178421596892070156, 40.17206517740157778, 94.75121379611699979 ) ) ;
#14623 = AXIS2_PLACEMENT_3D ( 'NONE', #8408, #14683, #16286 ) ;
#14624 = CARTESIAN_POINT ( 'NONE',  ( -3.628867371436363953, 48.69222599884265179, 93.57933879782399345 ) ) ;
#14625 = CARTESIAN_POINT ( 'NONE',  ( 7.864691922653266332, 47.81281597943210215, 78.56977997600147035 ) ) ;
#14626 = ORIENTED_EDGE ( 'NONE', *, *, #9128, .T. ) ;
#14627 = PLANE ( 'NONE',  #2016 ) ;
#14628 = ORIENTED_EDGE ( 'NONE', *, *, #6946, .F. ) ;
#14629 = B_SPLINE_CURVE_WITH_KNOTS ( 'NONE', 3,
 ( #10022, #1725, #11513, #7995, #20947, #114, #5104, #10126, #19679, #17986, #16502, #16606, #1919, #11409, #6593, #13100, #11822, #18297 ),
 .UNSPECIFIED., .F., .F.,
 ( 4, 2, 2, 2, 2, 2, 2, 2, 4 ),
 ( 0.000000000000000000, 0.0007228893211762224416, 0.0009036116514702782418, 0.001084333981764333934, 0.001445778642352450738, 0.001807223302940567326, 0.002168667963528683913, 0.002530112624116800935, 0.002891557284704917522 ),
 .UNSPECIFIED. ) ;
#14630 = CARTESIAN_POINT ( 'NONE',  ( 2.635245049009969254, 48.69372030666295359, 92.95433879953098710 ) ) ;
#14631 = EDGE_CURVE ( 'NONE', #16809, #7189, #15740, .T. ) ;
#14632 = FACE_BOUND ( 'NONE', #3425, .T. ) ;
#14633 = CARTESIAN_POINT ( 'NONE',  ( 9.294532183588495755, 42.65002709052886587, 79.09515810002898206 ) ) ;
#14634 = B_SPLINE_SURFACE_WITH_KNOTS ( 'NONE', 3, 1, ( 
 ( #4839, #13362 ),
 ( #8362, #11461 ),
 ( #19732, #6752 ),
 ( #5149, #18244 ),
 ( #11769, #5253 ),
 ( #16659, #3665 ),
 ( #14843, #19624 ),
 ( #18040, #6544 ),
 ( #3461, #5358 ),
 ( #16240, #475 ),
 ( #1874, #1776 ),
 ( #8257, #14743 ),
 ( #11670, #17930 ),
 ( #13258, #11565 ),
 ( #10176, #9973 ),
 ( #4939, #17826 ),
 ( #9755, #3353 ),
 ( #18147, #13459 ),
 ( #2080, #63 ),
 ( #164, #1973 ),
 ( #16454, #3566 ),
 ( #8575, #5045 ),
 ( #6647, #9863 ),
 ( #15062, #16346 ),
 ( #6953, #19931 ),
 ( #3256, #10072 ),
 ( #19832, #263 ) ),
 .UNSPECIFIED., .F., .F., .F.,
 ( 4, 1, 1, 1, 1, 1, 1, 1, 1, 1, 1, 1, 1, 1, 1, 1, 1, 1, 1, 1, 1, 1, 1, 1, 4 ),
 ( 2, 2 ),
 ( 0.000000000000000000, 0.06156270711109813193, 0.1195928175617291256, 0.1747495234496604655, 0.2265549029623682431, 0.2754357869405233972, 0.3212504303641821046, 0.3646692690278454108, 0.4055209537250142326, 0.4439801712034092684, 0.4803226396643038298, 0.5144678959723257838, 0.5464657104125147935, 0.5769957197620103617, 0.6058640933454703115, 0.6335754242279014736, 0.6604510950290067850, 0.6887476664015759198, 0.7209157586619387992, 0.7570169132788651112, 0.7970502319830404803, 0.8414026928090143631, 0.8898175437432860324, 0.9426652073923825759, 1.000000000000000000 ),
 ( 0.000000000000000000, 1.000000000000000000 ),
 .UNSPECIFIED. ) ;
#14635 = ORIENTED_EDGE ( 'NONE', *, *, #19129, .T. ) ;
#14636 = CARTESIAN_POINT ( 'NONE',  ( -1.077846259693496345, 47.82824192744436687, 77.55433879953099563 ) ) ;
#14637 = DIRECTION ( 'NONE',  ( -1.540237394707284220E-16, -1.793354297423764243E-16, 1.000000000000000000 ) ) ;
#14638 = ORIENTED_EDGE ( 'NONE', *, *, #12362, .F. ) ;
#14639 = CARTESIAN_POINT ( 'NONE',  ( 5.713366999337934793, 51.26805585685155364, 78.93442753446957738 ) ) ;
#14640 = CARTESIAN_POINT ( 'NONE',  ( 0.3326973149608342673, 52.96014171822455552, 72.45433879953087342 ) ) ;
#14641 = CARTESIAN_POINT ( 'NONE',  ( 6.102441102155617969, 43.42752260303680600, 94.55496379953098085 ) ) ;
#14642 = ORIENTED_EDGE ( 'NONE', *, *, #10781, .F. ) ;
#14643 = DIRECTION ( 'NONE',  ( -1.402518428993830937E-16, 1.000000000000000000, -3.469446951953617147E-16 ) ) ;
#14644 = CARTESIAN_POINT ( 'NONE',  ( -4.167066744307394544, 37.46026616392322950, 78.11020518223413944 ) ) ;
#14645 = ORIENTED_EDGE ( 'NONE', *, *, #12237, .F. ) ;
#14646 = DIRECTION ( 'NONE',  ( -0.7071067811865433539, -0.7071067811865516806, -1.146387601258591105E-16 ) ) ;
#14647 = CARTESIAN_POINT ( 'NONE',  ( 5.396517835962451493, 50.75616155517602834, 78.93669174070734584 ) ) ;
#14648 = CYLINDRICAL_SURFACE ( 'NONE', #7131, 8.199999999999995737 ) ;
#14649 = CARTESIAN_POINT ( 'NONE',  ( 6.339010289386230568, 49.88108541395529016, 75.76076839092205262 ) ) ;
#14650 = CARTESIAN_POINT ( 'NONE',  ( 0.8503282811412333775, 52.95606000782370870, 77.76169174070734869 ) ) ;
#14651 = DIRECTION ( 'NONE',  ( -0.9485903129789527988, 0.3165065846431829311, -8.934458285744989980E-17 ) ) ;
#14652 = CARTESIAN_POINT ( 'NONE',  ( -0.3208136495745970151, 40.36218137147969998, 46.22755528265711433 ) ) ;
#14653 = CARTESIAN_POINT ( 'NONE',  ( 7.894261924073310510, 40.81774634178594141, 79.41216397796385706 ) ) ;
#14654 = VERTEX_POINT ( 'NONE', #369 ) ;
#14655 = VECTOR ( 'NONE', #3707, 1000.000000000000000 ) ;
#14656 = CARTESIAN_POINT ( 'NONE',  ( -5.505078341044295165, 38.60214220976732236, 76.32343661933127521 ) ) ;
#14657 = CARTESIAN_POINT ( 'NONE',  ( 9.317552545512265638, 42.71902057559893962, 75.91044101036179370 ) ) ;
#14658 = CARTESIAN_POINT ( 'NONE',  ( 0.5915713968613122153, 52.96553219837200999, 77.38375056423674891 ) ) ;
#14659 = DIRECTION ( 'NONE',  ( 0.5941461771851693774, 0.8043570849667760481, 2.357623395011396791E-16 ) ) ;
#14660 = AXIS2_PLACEMENT_3D ( 'NONE', #13305, #3401, #8191 ) ;
#14661 = ORIENTED_EDGE ( 'NONE', *, *, #16600, .T. ) ;
#14662 = EDGE_CURVE ( 'NONE', #2157, #7787, #3449, .T. ) ;
#14663 = CARTESIAN_POINT ( 'NONE',  ( 5.826095025493096990, 51.18478820489261949, 78.92065061514911406 ) ) ;
#14664 = VERTEX_POINT ( 'NONE', #16764 ) ;
#14665 = CARTESIAN_POINT ( 'NONE',  ( -1.348357406114875312, 47.70104341108812918, 53.28382765310962554 ) ) ;
#14666 = DIRECTION ( 'NONE',  ( -0.5670994908670485835, 0.8236492988270761595, 6.036271672687166828E-17 ) ) ;
#14667 = CARTESIAN_POINT ( 'NONE',  ( -4.721994780338719444, 37.09540803149950250, 78.93613021445058564 ) ) ;
#14668 = CARTESIAN_POINT ( 'NONE',  ( -1.183761187420877548, 49.81017696809242068, 95.05433879953098142 ) ) ;
#14670 = ADVANCED_FACE ( 'NONE', ( #15164 ), #20358, .T. ) ;
#14669 = CARTESIAN_POINT ( 'NONE',  ( -7.077609990433001208, 44.22210830145579763, 72.45433879953085921 ) ) ;
#14671 = CARTESIAN_POINT ( 'NONE',  ( 10.77494014480653917, 42.96218137147968008, 61.40715055817103263 ) ) ;
#14673 = B_SPLINE_CURVE_WITH_KNOTS ( 'NONE', 3,
 ( #14074, #20555, #12480, #15791, #1493, #8878, #17061, #7980, #14465, #2488, #12066, #18547 ),
 .UNSPECIFIED., .F., .F.,
 ( 4, 2, 2, 2, 2, 4 ),
 ( 0.000000000000000000, 0.0001234850242348347618, 0.0002469700484696695235, 0.0004939400969393640921, 0.0007409101454090586064, 0.0009878801938787531208 ),
 .UNSPECIFIED. ) ;
#14672 = VECTOR ( 'NONE', #14932, 1000.000000000000000 ) ;
#14674 = CARTESIAN_POINT ( 'NONE',  ( 6.912263059922415742, 50.38247963137696672, 77.24227907682649175 ) ) ;
#14675 = DIRECTION ( 'NONE',  ( -1.402518428993831430E-16, 1.000000000000000000, -2.891205793294680792E-16 ) ) ;
#14676 = AXIS2_PLACEMENT_3D ( 'NONE', #6881, #5379, #8492 ) ;
#14677 = CARTESIAN_POINT ( 'NONE',  ( -4.567115856812060670, 47.10047254335474065, 93.30496380123798872 ) ) ;
#14678 = ORIENTED_EDGE ( 'NONE', *, *, #9653, .T. ) ;
#14679 = CARTESIAN_POINT ( 'NONE',  ( -5.300296504961807820, 38.45858271615729507, 79.28390783734228364 ) ) ;
#14680 = CARTESIAN_POINT ( 'NONE',  ( -5.761564881245698544, 50.48783832367244884, 78.87652712212219797 ) ) ;
#14681 = CARTESIAN_POINT ( 'NONE',  ( -4.865811501566803088, 37.20163965017978569, 78.83844719616611485 ) ) ;
#14682 = AXIS2_PLACEMENT_3D ( 'NONE', #7188, #2096, #10305 ) ;
#14683 = DIRECTION ( 'NONE',  ( -0.9999689119394086223, 0.007885122365275665235, -1.526048693634353392E-16 ) ) ;
#14684 = AXIS2_PLACEMENT_3D ( 'NONE', #7916, #139, #9834 ) ;
#14685 = CARTESIAN_POINT ( 'NONE',  ( 8.456021123984127641, 40.13695625074483786, 75.80967849220077426 ) ) ;
#14686 = VERTEX_POINT ( 'NONE', #15271 ) ;
#14687 = ORIENTED_EDGE ( 'NONE', *, *, #6198, .T. ) ;
#14688 = CARTESIAN_POINT ( 'NONE',  ( -0.3971402239501222176, 52.97438961391468126, 75.56421855115301867 ) ) ;
#14689 = CARTESIAN_POINT ( 'NONE',  ( 0.5221537403065014127, 44.16218137147968292, 76.16022115247204738 ) ) ;
#14690 = DIRECTION ( 'NONE',  ( -0.3165065846431824870, -0.9485903129789529098, 0.000000000000000000 ) ) ;
#14691 = PLANE ( 'NONE',  #16888 ) ;
#14692 = CARTESIAN_POINT ( 'NONE',  ( -1.842009727706052091, 49.28276247982005742, 92.45433879953100131 ) ) ;
#14693 = ORIENTED_EDGE ( 'NONE', *, *, #15324, .F. ) ;
#14694 = DIRECTION ( 'NONE',  ( -2.909222284125557203E-16, -0.7071067811865512365, 0.7071067811865439090 ) ) ;
#14695 = ORIENTED_EDGE ( 'NONE', *, *, #13030, .F. ) ;
#14696 = CARTESIAN_POINT ( 'NONE',  ( -4.524181921268124462, 40.28999182795290324, 92.28933880123798872 ) ) ;
#14697 =( BOUNDED_CURVE ( )  B_SPLINE_CURVE ( 3, ( #131, #19588, #3535, #14911 ),
 .UNSPECIFIED., .F., .F. ) 
 B_SPLINE_CURVE_WITH_KNOTS ( ( 4, 4 ),
 ( 1.230959417340772299, 1.276280841686757928 ),
 .UNSPECIFIED. ) 
 CURVE ( )  GEOMETRIC_REPRESENTATION_ITEM ( )  RATIONAL_B_SPLINE_CURVE ( ( 1.000000000000000000, 0.9998288380325437430, 0.9998288380325437430, 1.000000000000000000 ) ) 
 REPRESENTATION_ITEM ( '' )  );
#14698 = EDGE_CURVE ( 'NONE', #9268, #14408, #1119, .T. ) ;
#14699 = CARTESIAN_POINT ( 'NONE',  ( 1.332854164384612128, 52.20776918474795281, 76.79234737414994072 ) ) ;
#14700 = VECTOR ( 'NONE', #7911, 1000.000000000000000 ) ;
#14701 = CARTESIAN_POINT ( 'NONE',  ( 1.403788643848841833, 39.16218137147969003, 94.63983168766084475 ) ) ;
#14702 = VECTOR ( 'NONE', #2106, 1000.000000000000000 ) ;
#14703 = ADVANCED_FACE ( 'NONE', ( #7501, #5795, #11983, #15590, #13989, #10721 ), #20039, .T. ) ;
#14704 = CARTESIAN_POINT ( 'NONE',  ( 8.378637954445377289, 41.81363803720061867, 76.38301527011910252 ) ) ;
#14705 = CARTESIAN_POINT ( 'NONE',  ( 5.920503277122149299, 37.20387208676527280, 78.36928251986560667 ) ) ;
#14706 = EDGE_LOOP ( 'NONE', ( #15055, #17870, #11921, #5093 ) ) ;
#14707 = ADVANCED_FACE ( 'NONE', ( #3976 ), #18458, .T. ) ;
#14708 = EDGE_CURVE ( 'NONE', #18879, #16685, #15487, .T. ) ;
#14709 = ORIENTED_EDGE ( 'NONE', *, *, #4301, .F. ) ;
#14710 = CARTESIAN_POINT ( 'NONE',  ( 3.460444912181559474, 49.25145096859824889, 91.89871380123798872 ) ) ;
#14711 = CARTESIAN_POINT ( 'NONE',  ( -3.532917577324399261, 36.21708460058427193, 78.46683879953087626 ) ) ;
#14712 = EDGE_CURVE ( 'NONE', #2251, #12039, #2604, .T. ) ;
#14713 = ORIENTED_EDGE ( 'NONE', *, *, #15507, .F. ) ;
#14714 = CARTESIAN_POINT ( 'NONE',  ( 8.221644392715633742, 41.34114708762416512, 77.83751483520470060 ) ) ;
#14715 = CARTESIAN_POINT ( 'NONE',  ( 8.887668352622405621, 41.43063037816333605, 75.36022115247205022 ) ) ;
#14716 = AXIS2_PLACEMENT_3D ( 'NONE', #13847, #2477, #5763 ) ;
#14717 = CARTESIAN_POINT ( 'NONE',  ( 5.751194534584169737, 45.49804388114897336, 92.55433879953095300 ) ) ;
#14718 = CARTESIAN_POINT ( 'NONE',  ( -4.383592986664169189, 51.47248658876933547, 78.47566305278908771 ) ) ;
#14719 = CARTESIAN_POINT ( 'NONE',  ( 5.428747419638988880, 36.85248135533887393, 77.49967648550449439 ) ) ;
#14720 = EDGE_LOOP ( 'NONE', ( #2992, #12269, #19253, #15060 ) ) ;
#14721 = CARTESIAN_POINT ( 'NONE',  ( -4.051350930180527499, 50.96297916595425193, 76.10127045261064893 ) ) ;
#14722 = CARTESIAN_POINT ( 'NONE',  ( 4.135038682601217097, 47.90320695352507130, 92.55433879953098142 ) ) ;
#14723 = EDGE_LOOP ( 'NONE', ( #16580, #18004, #1234, #5934 ) ) ;
#14724 = CARTESIAN_POINT ( 'NONE',  ( 4.224453164177068842, 51.45384152454902704, 77.98100106196224601 ) ) ;
#14725 = CARTESIAN_POINT ( 'NONE',  ( 30.92220646078100188, 42.76218137147968434, 61.80715055817104542 ) ) ;
#14726 = CARTESIAN_POINT ( 'NONE',  ( 6.573693162767833442, 44.00881163587200717, 72.45433879953087342 ) ) ;
#14727 = CARTESIAN_POINT ( 'NONE',  ( 0.2860873169776692038, 38.75537135769874197, 95.84496379611699979 ) ) ;
#14728 = CARTESIAN_POINT ( 'NONE',  ( 4.673174852049362116, 39.63213674411673537, 92.95433879782399345 ) ) ;
#14729 = CARTESIAN_POINT ( 'NONE',  ( -5.389245695702297390, 49.84508174962770255, 72.45433879953087342 ) ) ;
#14730 = CARTESIAN_POINT ( 'NONE',  ( 8.107024659646262066, 47.29146611110563470, 76.48622618158429987 ) ) ;
#14731 = AXIS2_PLACEMENT_3D ( 'NONE', #7766, #15858, #1178 ) ;
#14732 = CARTESIAN_POINT ( 'NONE',  ( -3.509782604184575661, 36.19999572785944508, 77.03801799112748938 ) ) ;
#14733 = VERTEX_POINT ( 'NONE', #9101 ) ;
#14734 = EDGE_CURVE ( 'NONE', #7261, #12967, #13774, .T. ) ;
#14735 = CARTESIAN_POINT ( 'NONE',  ( 1.199929786271850540, 52.20873427653266674, 79.49721971971477785 ) ) ;
#14736 = CARTESIAN_POINT ( 'NONE',  ( 2.522153740306508407, 50.16218137147969713, 66.55433879953099563 ) ) ;
#14737 = ORIENTED_EDGE ( 'NONE', *, *, #3774, .T. ) ;
#14738 = CARTESIAN_POINT ( 'NONE',  ( 4.668432554735347573, 52.03990683855252541, 77.97037332800861975 ) ) ;
#14739 = CARTESIAN_POINT ( 'NONE',  ( 2.263363662449282110, 49.77488197367689793, 93.03606768333816035 ) ) ;
#14740 = CARTESIAN_POINT ( 'NONE',  ( 9.327624742576356098, 42.74920758916827168, 78.90414333341678343 ) ) ;
#14741 = ORIENTED_EDGE ( 'NONE', *, *, #913, .F. ) ;
#14742 = DIRECTION ( 'NONE',  ( 0.9534635866061451637, 0.3015081906286224411, 2.009271279954815058E-16 ) ) ;
#14743 = CARTESIAN_POINT ( 'NONE',  ( -5.623541984526494453, 37.76134463469641389, 75.60525969576029581 ) ) ;
#14744 = EDGE_LOOP ( 'NONE', ( #16114, #9323, #2141, #6522 ) ) ;
#14745 = PLANE ( 'NONE',  #6371 ) ;
#14746 = CARTESIAN_POINT ( 'NONE',  ( -4.517176205512261511, 36.94411680087065264, 76.50360254650976799 ) ) ;
#14747 = CARTESIAN_POINT ( 'NONE',  ( -2.077846259693550746, 39.65884927180063357, 96.66433879953098085 ) ) ;
#14748 = ORIENTED_EDGE ( 'NONE', *, *, #4151, .F. ) ;
#14749 = CARTESIAN_POINT ( 'NONE',  ( -4.806942593991916368, 37.15815555953845717, 77.31392376534303423 ) ) ;
#14750 = CARTESIAN_POINT ( 'NONE',  ( -4.517387068041375464, 36.94427255652680486, 78.31852111096432623 ) ) ;
#14751 = ORIENTED_EDGE ( 'NONE', *, *, #19223, .T. ) ;
#14752 = CARTESIAN_POINT ( 'NONE',  ( -4.762271096064603526, 51.20189707608225405, 76.05031124229590489 ) ) ;
#14753 = CARTESIAN_POINT ( 'NONE',  ( -3.154801521863568325, 47.83913663364971569, 83.28180655319408743 ) ) ;
#14754 = DIRECTION ( 'NONE',  ( 0.3165065846431827645, 0.9485903129789529098, 0.000000000000000000 ) ) ;
#14755 = CARTESIAN_POINT ( 'NONE',  ( -5.154188915835984375, 42.64120994080404614, 93.46121380123797451 ) ) ;
#14756 = DIRECTION ( 'NONE',  ( 0.000000000000000000, 0.000000000000000000, 1.000000000000000000 ) ) ;
#14757 = CARTESIAN_POINT ( 'NONE',  ( 6.780993214391527246, 50.47944337839869888, 75.76076839092205262 ) ) ;
#14758 = CARTESIAN_POINT ( 'NONE',  ( 8.797519961583052606, 41.16044993131110630, 77.39661844205990349 ) ) ;
#14759 = CARTESIAN_POINT ( 'NONE',  ( 5.288291328326708118, 36.75211657491283290, 75.39318197153889400 ) ) ;
#14760 = CARTESIAN_POINT ( 'NONE',  ( 7.726247110976633969, 40.31419528827419185, 79.00897045670630803 ) ) ;
#14761 = EDGE_LOOP ( 'NONE', ( #13507, #8533, #1393, #8978 ) ) ;
#14762 = CARTESIAN_POINT ( 'NONE',  ( -3.154801521863568325, 47.83913663364971569, 95.05036078214054385 ) ) ;
#14763 = PLANE ( 'NONE',  #18067 ) ;
#14764 = CARTESIAN_POINT ( 'NONE',  ( 5.740585635973908474, 51.24795054640212300, 75.97198585835440099 ) ) ;
#14765 = CARTESIAN_POINT ( 'NONE',  ( 6.197624760850954928, 49.99633915028627484, 77.73730439759678745 ) ) ;
#14766 = EDGE_LOOP ( 'NONE', ( #1753, #15806, #18226, #16505 ) ) ;
#14767 = DIRECTION ( 'NONE',  ( -0.8660254037844395958, 0.4999999999999983347, 0.000000000000000000 ) ) ;
#14768 = ORIENTED_EDGE ( 'NONE', *, *, #18206, .T. ) ;
#14769 = EDGE_CURVE ( 'NONE', #3265, #3130, #8783, .T. ) ;
#14770 = CARTESIAN_POINT ( 'NONE',  ( 31.07218010054375412, 42.76218137147968434, 65.80574467885102763 ) ) ;
#14771 = LINE ( 'NONE', #19451, #11806 ) ;
#14772 = CARTESIAN_POINT ( 'NONE',  ( -0.8591174924091972143, 52.85316264988993851, 76.01910742181597413 ) ) ;
#14773 = CARTESIAN_POINT ( 'NONE',  ( 5.404201196092212278, 50.75047497752489534, 79.54845644658969661 ) ) ;
#14774 = DIRECTION ( 'NONE',  ( -0.000000000000000000, -0.000000000000000000, 1.000000000000000000 ) ) ;
#14775 = CARTESIAN_POINT ( 'NONE',  ( -0.3080929418689875576, 37.85583172076932357, 93.69558880123807398 ) ) ;
#14776 = CARTESIAN_POINT ( 'NONE',  ( 4.539372959821318609, 52.13523796247791608, 76.58963291717793709 ) ) ;
#14777 = CARTESIAN_POINT ( 'NONE',  ( 4.356938870179031476, 51.41061492582127102, 77.85154143510365543 ) ) ;
#14778 = DIRECTION ( 'NONE',  ( -0.3165065846431824870, -0.9485903129789529098, 0.000000000000000000 ) ) ;
#14779 = B_SPLINE_CURVE_WITH_KNOTS ( 'NONE', 3,
 ( #2591, #7485, #9307, #7793, #14277, #20756, #2494, #6191, #12694, #8988, #19172, #13976, #8107, #13007, #17576, #3111, #8323, #20860, #14490 ),
 .UNSPECIFIED., .F., .F.,
 ( 4, 1, 1, 1, 1, 1, 1, 1, 1, 1, 1, 1, 1, 1, 1, 1, 4 ),
 ( 0.000000000000000000, 0.06114104454794499349, 0.1175581266966176375, 0.1702703359127188676, 0.2207833336891595610, 0.2680835234284920654, 0.3093802502289375589, 0.3470663877653532570, 0.3827844710311357757, 0.4080409699193555118, 0.4487658506906452294, 0.5030388115584650821, 0.5728007717267906695, 0.6580545229227713344, 0.7568648491070055773, 0.8711692811930628055, 1.000000000000000000 ),
 .UNSPECIFIED. ) ;
#14780 = EDGE_CURVE ( 'NONE', #14563, #8403, #17384, .T. ) ;
#14781 = CARTESIAN_POINT ( 'NONE',  ( -0.3080929418689875576, 37.85583172076933778, 93.69558880123800293 ) ) ;
#14782 = ORIENTED_EDGE ( 'NONE', *, *, #5329, .T. ) ;
#14783 = CARTESIAN_POINT ( 'NONE',  ( 28.43948732994508788, 43.16218137147969003, 74.70433879953100131 ) ) ;
#14784 = CARTESIAN_POINT ( 'NONE',  ( -5.569761608070843195, 50.62489392031717728, 79.19259575086972802 ) ) ;
#14785 = CARTESIAN_POINT ( 'NONE',  ( 8.349122434088485534, 41.71505415299095176, 75.36168763251107805 ) ) ;
#14786 = LINE ( 'NONE', #1607, #4430 ) ;
#14787 = CARTESIAN_POINT ( 'NONE',  ( 1.652727357819363974, 35.35299279957455099, 79.45433879953087342 ) ) ;
#14788 = ORIENTED_EDGE ( 'NONE', *, *, #8209, .F. ) ;
#14789 = CARTESIAN_POINT ( 'NONE',  ( 6.431452980651660489, 38.48875362012321943, 76.25518385353585415 ) ) ;
#14790 = EDGE_CURVE ( 'NONE', #5251, #18002, #20472, .T. ) ;
#14791 = CARTESIAN_POINT ( 'NONE',  ( -3.134114116279072881, 48.15229756555780227, 94.12621379611699979 ) ) ;
#14792 = CARTESIAN_POINT ( 'NONE',  ( -3.638656433990025807, 36.29518963458221492, 75.82994300095940332 ) ) ;
#14793 = CARTESIAN_POINT ( 'NONE',  ( -1.440187084481232338, 38.28092143101017797, 82.45433879953087342 ) ) ;
#14794 = VERTEX_POINT ( 'NONE', #18665 ) ;
#14795 = CARTESIAN_POINT ( 'NONE',  ( 5.202885763635528349, 50.89499265101085967, 72.45433879953087342 ) ) ;
#14796 = VERTEX_POINT ( 'NONE', #4085 ) ;
#14797 = CARTESIAN_POINT ( 'NONE',  ( 6.828503391016846891, 43.33193468930419101, 91.50808880123798872 ) ) ;
#14798 = CARTESIAN_POINT ( 'NONE',  ( 2.115006836158880521, 52.20160162348516764, 77.84551527011910821 ) ) ;
#14799 = DIRECTION ( 'NONE',  ( -1.110223024625156540E-16, -1.000000000000000000, -5.922860397471808077E-17 ) ) ;
#14800 = EDGE_CURVE ( 'NONE', #13025, #4092, #17097, .T. ) ;
#14801 = B_SPLINE_SURFACE_WITH_KNOTS ( 'NONE', 3, 1, ( 
 ( #7450, #12146 ),
 ( #17453, #18837 ),
 ( #2879, #17032 ),
 ( #2461, #963 ),
 ( #8955, #12256 ),
 ( #15441, #15547 ),
 ( #858, #7342 ),
 ( #13834, #20312 ),
 ( #13947, #5744 ),
 ( #20428, #18734 ),
 ( #9166, #15659 ),
 ( #17864, #16072 ),
 ( #9697, #3086 ),
 ( #4659, #1276 ),
 ( #6578, #20729 ),
 ( #14467, #3287 ),
 ( #6475, #13084 ),
 ( #17546, #1384 ),
 ( #9906, #17970 ),
 ( #7768, #7874 ),
 ( #1495, #14247 ),
 ( #6164, #8185 ),
 ( #9793, #17651 ) ),
 .UNSPECIFIED., .F., .F., .F.,
 ( 4, 1, 1, 1, 1, 1, 1, 1, 1, 1, 1, 1, 1, 1, 1, 1, 1, 1, 1, 1, 4 ),
 ( 2, 2 ),
 ( 0.000000000000000000, 0.05038957832574614271, 0.09924218466120336701, 0.1466944942679149211, 0.1933274803506509210, 0.2393051970681265017, 0.2845336341364397836, 0.3290963736026611408, 0.3737734709422849688, 0.4170414937111141529, 0.4581341819676884586, 0.4966705307863439889, 0.5335170563061359950, 0.5686625127317078698, 0.6026561223054673899, 0.6353294289861355360, 0.6676748031221235724, 0.7363421380907280156, 0.8138933404431207830, 0.9017813486866357309, 1.000000000000000000 ),
 ( 0.000000000000000000, 1.000000000000000000 ),
 .UNSPECIFIED. ) ;
#14802 = EDGE_CURVE ( 'NONE', #1396, #19108, #6000, .T. ) ;
#14803 = PLANE ( 'NONE',  #733 ) ;
#14804 = VERTEX_POINT ( 'NONE', #11224 ) ;
#14805 = DIRECTION ( 'NONE',  ( -0.9485903129789527988, 0.3165065846431829311, -8.934458285744989980E-17 ) ) ;
#14806 = VERTEX_POINT ( 'NONE', #4698 ) ;
#14807 = CARTESIAN_POINT ( 'NONE',  ( -3.154801521863568325, 47.83913663364971569, 92.86286078555453116 ) ) ;
#14808 = CARTESIAN_POINT ( 'NONE',  ( -1.677846259693481556, 44.16218137147969003, 54.55433879953098852 ) ) ;
#14809 = EDGE_CURVE ( 'NONE', #16100, #13896, #19475, .T. ) ;
#14810 = CARTESIAN_POINT ( 'NONE',  ( 4.394343283833276992, 39.11584570990505938, 95.10183880123797451 ) ) ;
#14811 = ORIENTED_EDGE ( 'NONE', *, *, #19884, .F. ) ;
#14812 = ADVANCED_FACE ( 'NONE', ( #20572 ), #17697, .T. ) ;
#14813 = DIRECTION ( 'NONE',  ( -0.9485903129789527988, 0.3165065846431829311, -8.934458285744989980E-17 ) ) ;
#14814 = EDGE_CURVE ( 'NONE', #3900, #10995, #6976, .T. ) ;
#14815 = CARTESIAN_POINT ( 'NONE',  ( 8.172753155408216230, 41.66916893826013535, 75.36022115247205022 ) ) ;
#14816 = CARTESIAN_POINT ( 'NONE',  ( 6.027795660425420365, 43.94244667862099618, 92.55433879953100984 ) ) ;
#14817 = CARTESIAN_POINT ( 'NONE',  ( -4.045487599862485517, 50.96716888712930427, 78.75145056212190298 ) ) ;
#14818 = EDGE_CURVE ( 'NONE', #20802, #374, #15700, .T. ) ;
#14819 = LINE ( 'NONE', #16321, #4127 ) ;
#14820 = EDGE_LOOP ( 'NONE', ( #12597, #6228, #5007, #1643 ) ) ;
#14821 = CARTESIAN_POINT ( 'NONE',  ( 11.22215374030650281, 51.36218137147968577, 62.80715055817104542 ) ) ;
#14822 = PRODUCT_DEFINITION ( 'UNKNOWN', '', #2070, #13828 ) ;
#14823 = ORIENTED_EDGE ( 'NONE', *, *, #15609, .T. ) ;
#14824 = DIRECTION ( 'NONE',  ( -5.626130192357176673E-16, -1.831515347669941892E-30, 1.000000000000000000 ) ) ;
#14825 = CARTESIAN_POINT ( 'NONE',  ( -6.770023921829650071, 40.50299573356667793, 77.79645048995966761 ) ) ;
#14826 = EDGE_CURVE ( 'NONE', #18462, #2266, #16376, .T. ) ;
#14827 = CARTESIAN_POINT ( 'NONE',  ( -5.835824771109036746, 39.98772221508849611, 72.45432679953087529 ) ) ;
#14828 = CARTESIAN_POINT ( 'NONE',  ( 9.026838159693451047, 41.84773111872319618, 78.13669174070733447 ) ) ;
#14829 = CARTESIAN_POINT ( 'NONE',  ( 5.666884522201896424, 41.76315400873614436, 91.78246379782397923 ) ) ;
#14830 = CARTESIAN_POINT ( 'NONE',  ( -7.079975527142585712, 43.92211762787398044, 72.45433879953085921 ) ) ;
#14831 = CARTESIAN_POINT ( 'NONE',  ( -7.725086623296537169, 47.24405475114629382, 77.94747975791852923 ) ) ;
#14832 = CARTESIAN_POINT ( 'NONE',  ( -4.472548095981605520, 51.40892252450552036, 75.36471306604558151 ) ) ;
#14833 = ORIENTED_EDGE ( 'NONE', *, *, #2302, .F. ) ;
#14834 = CARTESIAN_POINT ( 'NONE',  ( 0.5221537403065191763, 44.16218137147969003, 53.55433879953099563 ) ) ;
#14835 = CARTESIAN_POINT ( 'NONE',  ( 0.3821786226492928651, 35.36301154328572949, 75.45433879953087342 ) ) ;
#14836 = ORIENTED_EDGE ( 'NONE', *, *, #12873, .T. ) ;
#14837 = B_SPLINE_CURVE_WITH_KNOTS ( 'NONE', 3,
 ( #1270, #9271, #12451, #9474, #20832, #15761, #9372, #1176, #11077, #4654, #2873, #20526, #19047, #4456, #5853, #14139, #15960, #2659, #18931 ),
 .UNSPECIFIED., .F., .F.,
 ( 4, 1, 1, 1, 1, 1, 1, 1, 1, 1, 1, 1, 1, 1, 1, 1, 4 ),
 ( 0.000000000000000000, 0.1010931020334112918, 0.1936883160783454683, 0.2783829231069467891, 0.3553896825508546242, 0.4249031060497730494, 0.4877225005288854942, 0.5445694316561201509, 0.5961453798982884189, 0.6449762784811632343, 0.6930678288708707058, 0.7409100032456262808, 0.7895445362486890328, 0.8390228595812658785, 0.8900783947972482624, 0.9435774522572311085, 1.000000000000000000 ),
 .UNSPECIFIED. ) ;
#14838 = CYLINDRICAL_SURFACE ( 'NONE', #1028, 0.5999999999999894307 ) ;
#14839 = DIRECTION ( 'NONE',  ( -0.9485903129789495791, 0.3165065846431928120, -8.934458285744765648E-17 ) ) ;
#14840 = CARTESIAN_POINT ( 'NONE',  ( 1.256812508749381774, 49.74246873332880625, 94.86746379953099506 ) ) ;
#14841 = VERTEX_POINT ( 'NONE', #14185 ) ;
#14842 = CARTESIAN_POINT ( 'NONE',  ( 1.352400422481993658, 50.46853102219002096, 95.72683880123798872 ) ) ;
#14843 = CARTESIAN_POINT ( 'NONE',  ( -4.803777751955213837, 38.09182431430669880, 75.42164981362142839 ) ) ;
#14844 = ORIENTED_EDGE ( 'NONE', *, *, #15312, .F. ) ;
#14845 = LINE ( 'NONE', #4841, #10833 ) ;
#14846 = CARTESIAN_POINT ( 'NONE',  ( 0.3458533632374572453, 52.96041607507793714, 76.11020930090303693 ) ) ;
#14847 = EDGE_CURVE ( 'NONE', #16377, #2198, #12604, .T. ) ;
#14848 = CARTESIAN_POINT ( 'NONE',  ( -3.943187491250720544, 40.73580453397070755, 94.08621379953100927 ) ) ;
#14849 = ORIENTED_EDGE ( 'NONE', *, *, #6343, .F. ) ;
#14850 = FACE_OUTER_BOUND ( 'NONE', #4903, .T. ) ;
#14851 = VECTOR ( 'NONE', #14824, 1000.000000000000000 ) ;
#14852 = PRODUCT_DEFINITION_CONTEXT ( 'detailed design', #1243, 'design' ) ;
#14853 = ORIENTED_EDGE ( 'NONE', *, *, #412, .T. ) ;
#14854 = DIRECTION ( 'NONE',  ( 6.308085367188358884E-15, 8.847205979147994320E-31, 1.000000000000000000 ) ) ;
#14855 = CARTESIAN_POINT ( 'NONE',  ( 1.978191321044207474, 52.84097467239952550, 75.87687246405737085 ) ) ;
#14856 = EDGE_CURVE ( 'NONE', #9071, #3866, #4393, .T. ) ;
#14857 = LINE ( 'NONE', #6451, #11902 ) ;
#14858 = CARTESIAN_POINT ( 'NONE',  ( 0.6184261976043861075, 52.96580428404300989, 76.85126224504509196 ) ) ;
#14859 = ORIENTED_EDGE ( 'NONE', *, *, #5452, .F. ) ;
#14860 = CARTESIAN_POINT ( 'NONE',  ( 4.442698562174268062, 36.14788694334743013, 76.14998054923410109 ) ) ;
#14861 = VECTOR ( 'NONE', #19553, 1000.000000000000000 ) ;
#14862 = ORIENTED_EDGE ( 'NONE', *, *, #1693, .T. ) ;
#14863 = CARTESIAN_POINT ( 'NONE',  ( -5.185247867692305945, 38.27425900083883903, 75.57863954941232976 ) ) ;
#14864 = CARTESIAN_POINT ( 'NONE',  ( 9.204112107805267229, 42.37903238726386945, 75.57016332177543916 ) ) ;
#14865 = CARTESIAN_POINT ( 'NONE',  ( 5.591308205070052217, 40.32050054405898720, 80.55433879953099563 ) ) ;
#14866 = CARTESIAN_POINT ( 'NONE',  ( 26.43948732994507367, 43.16218137147969003, 74.70433879953098710 ) ) ;
#14867 = VERTEX_POINT ( 'NONE', #14401 ) ;
#14868 = DIRECTION ( 'NONE',  ( 0.3165065846431826535, 0.9485903129789529098, 2.188653791613874008E-16 ) ) ;
#14869 = VERTEX_POINT ( 'NONE', #2815 ) ;
#14870 = PLANE ( 'NONE',  #13187 ) ;
#14871 = VECTOR ( 'NONE', #18228, 1000.000000000000000 ) ;
#14872 = CARTESIAN_POINT ( 'NONE',  ( 9.353328126263708242, 42.82624226067153472, 76.54645538997905874 ) ) ;
#14873 = PLANE ( 'NONE',  #15891 ) ;
#14874 = DIRECTION ( 'NONE',  ( 1.000000000000000000, -0.000000000000000000, -0.000000000000000000 ) ) ;
#14875 = CARTESIAN_POINT ( 'NONE',  ( -1.876873622437039257, 39.01745058958429269, 92.71996379782397923 ) ) ;
#14876 = CARTESIAN_POINT ( 'NONE',  ( 2.043125170982144745, 38.48583871533720213, 93.77371380123807398 ) ) ;
#14877 = CARTESIAN_POINT ( 'NONE',  ( 4.192089982862425401, 51.46692896115924043, 75.88092117868445996 ) ) ;
#14878 = CARTESIAN_POINT ( 'NONE',  ( 4.143017335158133641, 51.51944627275094746, 78.46169174070733732 ) ) ;
#14879 = CARTESIAN_POINT ( 'NONE',  ( -4.524181921268124462, 40.28999182795290324, 91.03933880123798872 ) ) ;
#14880 = CARTESIAN_POINT ( 'NONE',  ( 4.394343283833276992, 39.11584570990505938, 92.60183880123797451 ) ) ;
#14881 = VERTEX_POINT ( 'NONE', #4499 ) ;
#14882 = CARTESIAN_POINT ( 'NONE',  ( 5.151473114414916843, 37.39086402708484513, 75.36221941035768168 ) ) ;
#14883 = VECTOR ( 'NONE', #14468, 1000.000000000000000 ) ;
#14884 = DIRECTION ( 'NONE',  ( 0.8136266022444372803, 0.5813877811927012917, 2.295812393977109100E-16 ) ) ;
#14885 = CARTESIAN_POINT ( 'NONE',  ( -4.492578824834620121, 37.68058364860989684, 78.86751516113972116 ) ) ;
#14886 = DIRECTION ( 'NONE',  ( 0.007885122365275663500, 0.9999689119394085113, 1.805443505845543142E-16 ) ) ;
#14887 = CARTESIAN_POINT ( 'NONE',  ( -7.885657102084565828, 41.56435211639550431, 79.54845644658969661 ) ) ;
#14888 = DIRECTION ( 'NONE',  ( -0.8136266022444372803, -0.5813877811927012917, -2.295812393977109100E-16 ) ) ;
#14889 = ORIENTED_EDGE ( 'NONE', *, *, #17525, .T. ) ;
#14890 = ORIENTED_EDGE ( 'NONE', *, *, #520, .F. ) ;
#14891 = LINE ( 'NONE', #19366, #13548 ) ;
#14892 = CARTESIAN_POINT ( 'NONE',  ( 6.418481717452356961, 38.47948483034925715, 77.68698088877128782 ) ) ;
#14893 = CARTESIAN_POINT ( 'NONE',  ( 4.100026115879673583, 51.54044873340893673, 76.58963291717793709 ) ) ;
#14894 = CARTESIAN_POINT ( 'NONE',  ( 0.8317120302326751480, 52.95673948731686664, 76.08306827724030086 ) ) ;
#14895 = VERTEX_POINT ( 'NONE', #12705 ) ;
#14896 = CARTESIAN_POINT ( 'NONE',  ( 8.940907051378230719, 41.59019013573462331, 76.11674899411023887 ) ) ;
#14897 = AXIS2_PLACEMENT_3D ( 'NONE', #7156, #10057, #14930 ) ;
#14898 = DIRECTION ( 'NONE',  ( 3.154042683594179442E-15, 4.423602989573997160E-31, -1.000000000000000000 ) ) ;
#14899 = ORIENTED_EDGE ( 'NONE', *, *, #17661, .F. ) ;
#14900 = CARTESIAN_POINT ( 'NONE',  ( -0.3080929418689875576, 37.85583172076933778, 91.19558880123798872 ) ) ;
#14901 = CARTESIAN_POINT ( 'NONE',  ( -7.831942942175630584, 41.38181678794802565, 78.91953837536544825 ) ) ;
#14902 = CARTESIAN_POINT ( 'NONE',  ( -3.603146387903926051, 36.26895979397031056, 78.01078865174693533 ) ) ;
#14903 = ADVANCED_FACE ( 'NONE', ( #11021 ), #19183, .F. ) ;
#14904 = CARTESIAN_POINT ( 'NONE',  ( -5.154188915835984375, 42.64120994080404614, 94.71121380123797451 ) ) ;
#14905 = CARTESIAN_POINT ( 'NONE',  ( 23.03948732994508575, 45.16218137147969003, 76.90433879953100416 ) ) ;
#14906 = ORIENTED_EDGE ( 'NONE', *, *, #10316, .T. ) ;
#14907 = DIRECTION ( 'NONE',  ( 0.000000000000000000, 0.000000000000000000, 1.000000000000000000 ) ) ;
#14908 = AXIS2_PLACEMENT_3D ( 'NONE', #14479, #17257, #10894 ) ;
#14909 = VERTEX_POINT ( 'NONE', #4596 ) ;
#14910 = B_SPLINE_CURVE_WITH_KNOTS ( 'NONE', 3,
 ( #8696, #5488, #10513, #16980, #16568, #15176, #6764, #20056, #1989, #13275, #12003, #18474, #5165, #10410 ),
 .UNSPECIFIED., .F., .F.,
 ( 4, 2, 2, 2, 2, 2, 4 ),
 ( 0.000000000000000000, 0.0002739962706728955389, 0.0005479925413457910777, 0.0008219888120186866166, 0.001095985082691582155, 0.001643977624037381473, 0.002191970165383179923 ),
 .UNSPECIFIED. ) ;
#14911 = CARTESIAN_POINT ( 'NONE',  ( -1.219503646467430036, 49.90383875825363447, 69.41268141275705261 ) ) ;
#14912 = LINE ( 'NONE', #19590, #13564 ) ;
#14913 = ORIENTED_EDGE ( 'NONE', *, *, #2750, .F. ) ;
#14914 = DIRECTION ( 'NONE',  ( -0.5813877811926938532, 0.8136266022444424983, 5.636455622144827492E-17 ) ) ;
#14915 = CARTESIAN_POINT ( 'NONE',  ( 8.740212021938845055, 40.98869440064952130, 75.38759329643264095 ) ) ;
#14916 = CARTESIAN_POINT ( 'NONE',  ( 5.937214047150960461, 51.10270905974117994, 76.26580079864017137 ) ) ;
#14917 = EDGE_CURVE ( 'NONE', #17731, #16572, #16006, .T. ) ;
#14918 = DIRECTION ( 'NONE',  ( 1.000000000000000000, 0.000000000000000000, 0.000000000000000000 ) ) ;
#14919 = CARTESIAN_POINT ( 'NONE',  ( 0.4211168079077332038, 52.35552251280865477, 78.89168391585492657 ) ) ;
#14920 = VERTEX_POINT ( 'NONE', #14502 ) ;
#14921 = CARTESIAN_POINT ( 'NONE',  ( -4.423683986466107498, 51.44383902813605403, 76.03815620566271605 ) ) ;
#14922 = VECTOR ( 'NONE', #7334, 1000.000000000000114 ) ;
#14923 = ORIENTED_EDGE ( 'NONE', *, *, #14534, .F. ) ;
#14924 = DIRECTION ( 'NONE',  ( 0.5773502691896226224, 0.5773502691896224004, -0.5773502691896322814 ) ) ;
#14925 = CARTESIAN_POINT ( 'NONE',  ( -7.457252456121344686, 40.19216126113897758, 77.97023824993468111 ) ) ;
#14926 = EDGE_CURVE ( 'NONE', #2580, #13095, #20870, .T. ) ;
#14927 = VECTOR ( 'NONE', #6879, 1000.000000000000000 ) ;
#14928 = CARTESIAN_POINT ( 'NONE',  ( -6.210882734309923769, 46.73118581782181025, 75.45433879953087342 ) ) ;
#14929 = CARTESIAN_POINT ( 'NONE',  ( 5.053692675489762642, 42.04909006277621586, 92.32933879611698558 ) ) ;
#14930 = DIRECTION ( 'NONE',  ( 0.3165065846431826535, 0.9485903129789529098, 2.188653791613874008E-16 ) ) ;
#14931 = CARTESIAN_POINT ( 'NONE',  ( -3.628867371436365730, 48.69222599884265179, 94.82933879782397923 ) ) ;
#14932 = DIRECTION ( 'NONE',  ( 0.000000000000000000, 0.000000000000000000, 1.000000000000000000 ) ) ;
#14934 = ADVANCED_FACE ( 'NONE', ( #16429 ), #8435, .T. ) ;
#14933 = CARTESIAN_POINT ( 'NONE',  ( -7.087950778502929872, 47.02707019024424540, 77.87251963618699335 ) ) ;
#14935 = AXIS2_PLACEMENT_3D ( 'NONE', #4321, #7313, #16892 ) ;
#14936 = CLOSED_SHELL ( 'NONE', ( #5684, #6462, #20337, #5145, #14558, #16775, #16301, #5962, #14703, #18753, #5595, #9132, #7968, #3140, #14173, #1195, #2856, #8860, #382, #1009, #20101, #14560, #11715, #15481, #10839, #6248, #5977, #2129, #8997, #13530, #20512, #11059, #14566, #11630, #7266, #10584, #11548, #10711, #13425, #7304, #17184, #14286, #7821, #14588, #16393, #5825, #16802, #1254, #5600, #9321, #8628, #5707, #13520, #8196, #12200, #6994, #8349, #4740, #18985, #10807, #6891, #13221, #20317, #2276, #7697, #12102, #10574, #15584, #10516, #19225, #13614, #2756, #7186, #20126, #6299, #13951, #15001, #13941, #18740, #12769, #17034, #13271, #16830, #17895, #15754, #5091, #8559, #17558, #9715, #17404, #9351, #2711, #7149, #6089, #4949, #20486, #4366, #4893, #9798, #2061, #2753, #15022, #18404, #18235, #20797, #1792, #8736, #5408, #4899, #1077, #4251, #5703, #11184, #6971, #6495, #10543, #4545, #20170, #14167, #15842, #18842, #8105, #7277, #4517, #12638, #15895, #10542, #9280, #15638, #18592, #20834, #16664, #20938, #11476, #6612, #683, #15470, #18596, #1054, #6817, #14707, #10913, #12086, #4505, #14298, #1523, #3481, #5314, #9947, #5176, #10958, #4865, #7309, #13903, #8985, #12721, #5207, #1947, #19076, #8556, #10303, #15765, #18894, #4306, #12618, #6969, #3911, #3007, #2597, #15077, #1727, #6394, #3653, #257, #2361, #10038, #3892, #1573, #9255, #6088, #10437, #10970, #17299, #10538, #153, #5440, #14527, #18331, #15863, #3271, #1136, #11444, #10986, #20885, #1500, #18822, #6123, #8666, #4137, #8636, #17715, #16076, #11926, #1701, #21029, #12406, #2490, #923, #14071, #7668, #5481, #8678, #11400, #383, #10180, #4943, #9898, #11373, #15092, #3940, #14031, #20374, #19744, #11179 ) ) ;
#14937 = VERTEX_POINT ( 'NONE', #9944 ) ;
#14938 = CARTESIAN_POINT ( 'NONE',  ( -1.769308508470985863, 51.40850462968639079, 75.45433879953087342 ) ) ;
#14939 = CARTESIAN_POINT ( 'NONE',  ( 5.092481412199395763, 37.36999664754328876, 78.16244716952144245 ) ) ;
#14940 = ORIENTED_EDGE ( 'NONE', *, *, #13177, .T. ) ;
#14941 = DIRECTION ( 'NONE',  ( 0.000000000000000000, -1.000000000000000000, 2.168404344970984808E-15 ) ) ;
#14942 = EDGE_CURVE ( 'NONE', #12487, #6196, #1748, .T. ) ;
#14943 = DIRECTION ( 'NONE',  ( 9.598494438985367424E-18, -5.922860397471809309E-17, 1.000000000000000000 ) ) ;
#14944 = CARTESIAN_POINT ( 'NONE',  ( -3.943187491250720544, 40.73580453397070755, 95.33621379953099506 ) ) ;
#14945 = VECTOR ( 'NONE', #17190, 1000.000000000000000 ) ;
#14946 = ORIENTED_EDGE ( 'NONE', *, *, #10339, .F. ) ;
#14947 = AXIS2_PLACEMENT_3D ( 'NONE', #13115, #6824, #18114 ) ;
#14948 = DIRECTION ( 'NONE',  ( 1.000000000000000000, 1.402518428993831676E-16, 1.213361030872719641E-32 ) ) ;
#14949 = DIRECTION ( 'NONE',  ( -1.000000000000000000, 0.000000000000000000, 0.000000000000000000 ) ) ;
#14950 = ORIENTED_EDGE ( 'NONE', *, *, #12839, .F. ) ;
#14951 = FACE_OUTER_BOUND ( 'NONE', #16628, .T. ) ;
#14952 = CARTESIAN_POINT ( 'NONE',  ( 0.5234039149397815560, 52.96221744815497345, 75.97427060055225922 ) ) ;
#14953 = VERTEX_POINT ( 'NONE', #3541 ) ;
#14954 = VECTOR ( 'NONE', #10302, 1000.000000000000000 ) ;
#14955 = CARTESIAN_POINT ( 'NONE',  ( -3.944959226007136888, 38.51060946023304865, 77.05433879953086773 ) ) ;
#14956 = CARTESIAN_POINT ( 'NONE',  ( 1.352400422481993658, 50.46853102219002096, 94.47683880123798872 ) ) ;
#14957 = VECTOR ( 'NONE', #15146, 1000.000000000000000 ) ;
#14958 = ORIENTED_EDGE ( 'NONE', *, *, #13422, .T. ) ;
#14959 = CARTESIAN_POINT ( 'NONE',  ( 0.8337132176892476654, 52.35626200026493393, 77.58758220374809866 ) ) ;
#14960 = CARTESIAN_POINT ( 'NONE',  ( 1.725557703326630499, 52.87986937373156593, 75.61804811561941619 ) ) ;
#14961 = CARTESIAN_POINT ( 'NONE',  ( 5.611423337425062385, 41.22389019960463230, 95.17996380123798872 ) ) ;
#14962 = CARTESIAN_POINT ( 'NONE',  ( 0.000000000000000000, 0.000000000000000000, 0.000000000000000000 ) ) ;
#14963 = CARTESIAN_POINT ( 'NONE',  ( 6.695638642021790155, 50.54249136271632636, 75.66183449524544358 ) ) ;
#14964 = CIRCLE ( 'NONE', #15310, 3.999999999999996447 ) ;
#14966 = EDGE_CURVE ( 'NONE', #20991, #7197, #19495, .T. ) ;
#14965 = CARTESIAN_POINT ( 'NONE',  ( 5.467682621026056289, 50.70306757362737926, 77.28284099877059532 ) ) ;
#14967 = CARTESIAN_POINT ( 'NONE',  ( -7.203865160062882467, 41.41469608315769335, 78.54945882271483981 ) ) ;
#14968 = ORIENTED_EDGE ( 'NONE', *, *, #1419, .T. ) ;
#14969 = EDGE_CURVE ( 'NONE', #597, #20036, #1408, .T. ) ;
#14970 = VERTEX_POINT ( 'NONE', #234 ) ;
#14971 = DIRECTION ( 'NONE',  ( -1.000000000000000000, 0.000000000000000000, 0.000000000000000000 ) ) ;
#14972 = CARTESIAN_POINT ( 'NONE',  ( 7.676901518817963677, 40.16630341814867933, 78.16120960217517677 ) ) ;
#14973 = CIRCLE ( 'NONE', #4748, 3.199999999999987743 ) ;
#14974 = VERTEX_POINT ( 'NONE', #8119 ) ;
#14975 = FACE_OUTER_BOUND ( 'NONE', #10934, .T. ) ;
#14976 = EDGE_CURVE ( 'NONE', #1479, #15007, #19594, .T. ) ;
#14977 = CARTESIAN_POINT ( 'NONE',  ( -1.477846259693491149, 49.76218137147969856, 61.55433879953100273 ) ) ;
#14978 =( REPRESENTATION_RELATIONSHIP ('NONE','NONE', #11365, #333 ) REPRESENTATION_RELATIONSHIP_WITH_TRANSFORMATION ( #15604 )SHAPE_REPRESENTATION_RELATIONSHIP( ) );
#14979 = ORIENTED_EDGE ( 'NONE', *, *, #17423, .T. ) ;
#14980 = ORIENTED_EDGE ( 'NONE', *, *, #10415, .F. ) ;
#14981 = EDGE_CURVE ( 'NONE', #19783, #16684, #8228, .T. ) ;
#14982 = CARTESIAN_POINT ( 'NONE',  ( 1.514255888186008425, 52.36218137147968577, 52.53721119516358584 ) ) ;
#14983 = CARTESIAN_POINT ( 'NONE',  ( 6.103551234968451311, 50.05500953258444952, 77.68963291717794561 ) ) ;
#14984 = ORIENTED_EDGE ( 'NONE', *, *, #11811, .F. ) ;
#14985 = CARTESIAN_POINT ( 'NONE',  ( -3.495065479208315562, 36.18912478048144266, 76.62933879953087057 ) ) ;
#14986 = CARTESIAN_POINT ( 'NONE',  ( -1.077846259693496123, 50.16218137147969713, 77.55433879953099563 ) ) ;
#14987 = CARTESIAN_POINT ( 'NONE',  ( -3.167417508397908588, 51.48567728911131525, 79.16276250595325337 ) ) ;
#14988 = CARTESIAN_POINT ( 'NONE',  ( 0.002918113473574554962, 52.94761665455641975, 75.41770058766584839 ) ) ;
#14989 = CARTESIAN_POINT ( 'NONE',  ( -4.007890887056451135, 40.01116025973682611, 92.64183879782400766 ) ) ;
#14990 = B_SPLINE_SURFACE_WITH_KNOTS ( 'NONE', 3, 1, ( 
 ( #3276, #9573 ),
 ( #16261, #8170 ),
 ( #4962, #9994 ),
 ( #11483, #6565 ),
 ( #11276, #7967 ),
 ( #21022, #14452 ),
 ( #12854, #1585 ),
 ( #17958, #5172 ),
 ( #1800, #4751 ),
 ( #84, #6667 ),
 ( #1893, #6771 ),
 ( #14657, #14557 ),
 ( #19645, #13071 ),
 ( #16370, #19443 ),
 ( #16472, #8381 ),
 ( #14864, #281 ),
 ( #13281, #18167 ),
 ( #1995, #8490 ),
 ( #16574, #3584 ),
 ( #10091, #3458 ),
 ( #17722, #19306 ),
 ( #9655, #6428 ),
 ( #13047, #9858 ) ),
 .UNSPECIFIED., .F., .F., .F.,
 ( 4, 1, 1, 1, 1, 1, 1, 1, 1, 1, 1, 1, 1, 1, 1, 1, 1, 1, 1, 1, 4 ),
 ( 2, 2 ),
 ( 0.000000000000000000, 0.04300144207505136179, 0.08353165498080591944, 0.1209955408344369626, 0.1553840623654753617, 0.1873435814759382700, 0.2162479910858959298, 0.2424976236983500399, 0.2660452007499324312, 0.3104933729322157387, 0.3556083049253406791, 0.4034864083407884716, 0.4540969056831142825, 0.5078508224766279389, 0.5647468969590679899, 0.6259022191770886590, 0.6917657563094725681, 0.7621492621511971599, 0.8365553829333508551, 0.9158190838930461153, 1.000000000000000000 ),
 ( 0.000000000000000000, 1.000000000000000000 ),
 .UNSPECIFIED. ) ;
#14991 = FACE_OUTER_BOUND ( 'NONE', #11931, .T. ) ;
#14992 = DIRECTION ( 'NONE',  ( -0.8033560671169786005, -0.5954989751681698529, -2.305299702067830011E-16 ) ) ;
#14993 = DIRECTION ( 'NONE',  ( 0.3165065846431826535, 0.9485903129789529098, 2.188653791613874008E-16 ) ) ;
#14994 = CARTESIAN_POINT ( 'NONE',  ( 5.146041124512939824, 40.41782456190201600, 90.15009067557426192 ) ) ;
#14995 = CARTESIAN_POINT ( 'NONE',  ( -5.154188915835984375, 42.64120994080404614, 93.46121380123797451 ) ) ;
#14996 = VERTEX_POINT ( 'NONE', #17802 ) ;
#14997 = CARTESIAN_POINT ( 'NONE',  ( 3.962887037559272407, 36.71897260862575507, 76.53559901244523189 ) ) ;
#14998 = AXIS2_PLACEMENT_3D ( 'NONE', #19251, #1390, #4664 ) ;
#14999 = DIRECTION ( 'NONE',  ( -0.9534635866061451637, -0.3015081906286224411, -2.009271279954815058E-16 ) ) ;
#15000 = CARTESIAN_POINT ( 'NONE',  ( -8.190409139795066906, 42.92474528817020740, 76.06610350541322418 ) ) ;
#15001 = ADVANCED_FACE ( 'NONE', ( #19807 ), #3325, .T. ) ;
#15002 = CARTESIAN_POINT ( 'NONE',  ( -4.895222749246778804, 37.22336455408366618, 78.59503622499423159 ) ) ;
#15003 = CARTESIAN_POINT ( 'NONE',  ( 1.256812508749381774, 49.74246873332880625, 91.11746379953096664 ) ) ;
#15004 = CARTESIAN_POINT ( 'NONE',  ( 8.356946452252621782, 41.76007885337365622, 77.44430071719698105 ) ) ;
#15005 = DIRECTION ( 'NONE',  ( 1.540237394707284220E-16, 1.793354297423764243E-16, -1.000000000000000000 ) ) ;
#15006 = CARTESIAN_POINT ( 'NONE',  ( -0.2125050281363792815, 38.58189400963056670, 93.30496380294499659 ) ) ;
#15007 = VERTEX_POINT ( 'NONE', #6829 ) ;
#15008 = ORIENTED_EDGE ( 'NONE', *, *, #12906, .T. ) ;
#15009 = VECTOR ( 'NONE', #3652, 1000.000000000000114 ) ;
#15010 = DIRECTION ( 'NONE',  ( 0.3165065846431827645, 0.9485903129789529098, 0.000000000000000000 ) ) ;
#15011 = PLANE ( 'NONE',  #11793 ) ;
#15012 = LINE ( 'NONE', #8737, #8239 ) ;
#15013 = ORIENTED_EDGE ( 'NONE', *, *, #19975, .F. ) ;
#15014 = VECTOR ( 'NONE', #20918, 1000.000000000000000 ) ;
#15015 =( BOUNDED_CURVE ( )  B_SPLINE_CURVE ( 2, ( #19555, #3388, #11496, #8504, #17968 ),
 .UNSPECIFIED., .F., .F. ) 
 B_SPLINE_CURVE_WITH_KNOTS ( ( 3, 2, 3 ),
 ( 0.2430974982970244558, 0.2604082588139463583, 0.2691383253928207320 ),
 .UNSPECIFIED. ) 
 CURVE ( )  GEOMETRIC_REPRESENTATION_ITEM ( )  RATIONAL_B_SPLINE_CURVE ( ( 0.9660722094251257275, 0.9493985640419095873, 1.000000000000000000, 0.9744809649195396162, 0.9660722070857166166 ) ) 
 REPRESENTATION_ITEM ( '' )  );
#15016 = CARTESIAN_POINT ( 'NONE',  ( -1.579458713576543882, 38.67424504380988282, 95.05433879952670395 ) ) ;
#15017 = CARTESIAN_POINT ( 'NONE',  ( -5.968382836370076383, 47.45797339585421071, 78.32492703482499508 ) ) ;
#15018 = ORIENTED_EDGE ( 'NONE', *, *, #5720, .T. ) ;
#15019 = CARTESIAN_POINT ( 'NONE',  ( -5.058133621542618030, 44.89684013992257405, 95.49246380294496817 ) ) ;
#15020 = CARTESIAN_POINT ( 'NONE',  ( 1.700675709985738804, 52.20486877668423631, 76.92027168626151479 ) ) ;
#15021 = CARTESIAN_POINT ( 'NONE',  ( -3.108234509380449762, 36.81740333079968508, 78.23707788297487298 ) ) ;
#15022 = ADVANCED_FACE ( 'NONE', ( #10150 ), #2432, .T. ) ;
#15023 = CARTESIAN_POINT ( 'NONE',  ( 6.198496396448986090, 45.68315280215533392, 94.08621380123798872 ) ) ;
#15024 = CIRCLE ( 'NONE', #18089, 4.200000000000001066 ) ;
#15025 = CARTESIAN_POINT ( 'NONE',  ( 8.433872151619121738, 42.00521257461706170, 79.52184654923091500 ) ) ;
#15026 = EDGE_LOOP ( 'NONE', ( #824, #17211, #8697, #13901, #2929 ) ) ;
#15027 = VECTOR ( 'NONE', #855, 1000.000000000000000 ) ;
#15028 = DIRECTION ( 'NONE',  ( -0.3015081906286169455, 0.9534635866061470511, 1.245503830460480420E-16 ) ) ;
#15029 = ORIENTED_EDGE ( 'NONE', *, *, #3240, .T. ) ;
#15030 = CARTESIAN_POINT ( 'NONE',  ( -4.340948238162491535, 40.55733868359232730, 72.45433879953085921 ) ) ;
#15031 = CARTESIAN_POINT ( 'NONE',  ( 2.043125170982144745, 38.48583871533720213, 91.27371380123798872 ) ) ;
#15032 = ORIENTED_EDGE ( 'NONE', *, *, #11596, .F. ) ;
#15033 = DIRECTION ( 'NONE',  ( 0.5735764363510446051, 0.8191520442889927978, 9.299032798180135705E-17 ) ) ;
#15034 = CARTESIAN_POINT ( 'NONE',  ( 1.119863296874945791, 50.25084051303456789, 69.06567965797609077 ) ) ;
#15035 = DIRECTION ( 'NONE',  ( 1.540237394707284220E-16, 1.793354297423764243E-16, -1.000000000000000000 ) ) ;
#15036 = CARTESIAN_POINT ( 'NONE',  ( 0.3327559098722669417, 52.96757255913198748, 78.50066232894263862 ) ) ;
#15037 = ORIENTED_EDGE ( 'NONE', *, *, #18817, .F. ) ;
#15038 = PLANE ( 'NONE',  #1709 ) ;
#15039 = EDGE_CURVE ( 'NONE', #8376, #9835, #2534, .T. ) ;
#15040 = VECTOR ( 'NONE', #10287, 1000.000000000000000 ) ;
#15041 = ORIENTED_EDGE ( 'NONE', *, *, #8442, .F. ) ;
#15042 = DIRECTION ( 'NONE',  ( -0.3165065846431971419, -0.9485903129789481358, 0.000000000000000000 ) ) ;
#15043 = CARTESIAN_POINT ( 'NONE',  ( -7.537584518443389392, 40.44619647026995324, 77.53559663939034863 ) ) ;
#15044 = VECTOR ( 'NONE', #14874, 1000.000000000000000 ) ;
#15045 = DIRECTION ( 'NONE',  ( 1.540237394707284220E-16, 1.793354297423764243E-16, -1.000000000000000000 ) ) ;
#15046 = CARTESIAN_POINT ( 'NONE',  ( -3.098709854545130593, 36.80491647020841128, 78.46683879953087626 ) ) ;
#15047 = CARTESIAN_POINT ( 'NONE',  ( -4.622577041588897373, 46.56120873422322859, 94.90746379782396502 ) ) ;
#15048 = CARTESIAN_POINT ( 'NONE',  ( 2.522153740306509295, 47.62628298661744708, 61.15433879953099705 ) ) ;
#15049 = B_SPLINE_CURVE_WITH_KNOTS ( 'NONE', 3,
 ( #15686, #5892, #20653, #15795, #887, #5783, #7693, #17270, #15577, #2692, #992, #6083, #18768, #19079, #4182, #4585 ),
 .UNSPECIFIED., .F., .F.,
 ( 4, 2, 2, 2, 2, 2, 2, 4 ),
 ( 0.000000000000000000, 0.0001355735443734605323, 0.0002711470887469210646, 0.0004067206331203815427, 0.0005422941774938421292, 0.0006778677218673026614, 0.0008134412662407630853, 0.001084588354987687294 ),
 .UNSPECIFIED. ) ;
#15050 = ADVANCED_FACE ( 'NONE', ( #18910 ), #9997, .F. ) ;
#15051 = EDGE_CURVE ( 'NONE', #8901, #3406, #897, .T. ) ;
#15052 = ORIENTED_EDGE ( 'NONE', *, *, #5739, .F. ) ;
#15053 = CYLINDRICAL_SURFACE ( 'NONE', #3377, 8.199999999999995737 ) ;
#15054 = CARTESIAN_POINT ( 'NONE',  ( 1.083001295814570053, 52.34297901104275041, 76.77198585835439815 ) ) ;
#15055 = ORIENTED_EDGE ( 'NONE', *, *, #2596, .F. ) ;
#15056 = VECTOR ( 'NONE', #20067, 1000.000000000000114 ) ;
#15057 = DIRECTION ( 'NONE',  ( 0.000000000000000000, 0.000000000000000000, 1.000000000000000000 ) ) ;
#15058 = CARTESIAN_POINT ( 'NONE',  ( 3.948530577815480225, 39.69684013992245752, 95.64871379953100927 ) ) ;
#15059 = CARTESIAN_POINT ( 'NONE',  ( 5.025485839985549319, 41.56218137147963887, 94.47683879953099506 ) ) ;
#15060 = ORIENTED_EDGE ( 'NONE', *, *, #19181, .T. ) ;
#15061 = LINE ( 'NONE', #3565, #5433 ) ;
#15062 = CARTESIAN_POINT ( 'NONE',  ( -5.503510928868301733, 38.60868902512070377, 76.46818962967083166 ) ) ;
#15063 = EDGE_LOOP ( 'NONE', ( #15177, #5128, #227, #311 ) ) ;
#15064 = CARTESIAN_POINT ( 'NONE',  ( 5.614631715549363022, 51.34098763368633911, 78.82175487302160377 ) ) ;
#15065 = DIRECTION ( 'NONE',  ( -0.000000000000000000, 1.000000000000000000, -0.000000000000000000 ) ) ;
#15066 = ORIENTED_EDGE ( 'NONE', *, *, #783, .T. ) ;
#15067 = DIRECTION ( 'NONE',  ( 1.540237394707284220E-16, 1.793354297423764243E-16, -1.000000000000000000 ) ) ;
#15068 = CARTESIAN_POINT ( 'NONE',  ( -4.567115856812060670, 47.10047254335474065, 95.96121380123798872 ) ) ;
#15069 = ORIENTED_EDGE ( 'NONE', *, *, #1298, .T. ) ;
#15070 = CARTESIAN_POINT ( 'NONE',  ( -4.788785806866687089, 51.18295063450860738, 76.15325518536063498 ) ) ;
#15071 = DIRECTION ( 'NONE',  ( 1.000000000000000000, 4.924280921909908032E-16, 5.626130192357177659E-16 ) ) ;
#15072 = VECTOR ( 'NONE', #612, 1000.000000000000000 ) ;
#15073 = CARTESIAN_POINT ( 'NONE',  ( -0.2076320057883534465, -2.375669546006914178E-15, -16.19718824135994595 ) ) ;
#15074 = CARTESIAN_POINT ( 'NONE',  ( 6.298904310734356748, 49.91071008481807070, 75.70960632971019777 ) ) ;
#15075 = CARTESIAN_POINT ( 'NONE',  ( 0.4896586383660414543, 52.96222063074647224, 78.92934190660548666 ) ) ;
#15076 = CARTESIAN_POINT ( 'NONE',  ( 31.22215374030650281, 42.96218137147968008, 74.20433879953100131 ) ) ;
#15077 = ADVANCED_FACE ( 'NONE', ( #7500 ), #11767, .T. ) ;
#15078 = ORIENTED_EDGE ( 'NONE', *, *, #18480, .F. ) ;
#15079 = VERTEX_POINT ( 'NONE', #16317 ) ;
#15080 = CARTESIAN_POINT ( 'NONE',  ( 3.965773623613683796, 36.72686942586689440, 76.47837415541054895 ) ) ;
#15081 = CARTESIAN_POINT ( 'NONE',  ( 7.825649284229865721, 40.61210990747041905, 79.30521328845429707 ) ) ;
#15082 = ORIENTED_EDGE ( 'NONE', *, *, #14317, .F. ) ;
#15083 = LINE ( 'NONE', #16884, #13236 ) ;
#15084 = DIRECTION ( 'NONE',  ( 1.540237394707284220E-16, 1.793354297423764243E-16, -1.000000000000000000 ) ) ;
#15085 = CARTESIAN_POINT ( 'NONE',  ( 1.352400422481993658, 50.46853102219002096, 93.22683880123798872 ) ) ;
#15086 = ORIENTED_EDGE ( 'NONE', *, *, #16653, .T. ) ;
#15087 = ORIENTED_EDGE ( 'NONE', *, *, #16162, .T. ) ;
#15088 = VECTOR ( 'NONE', #14799, 1000.000000000000000 ) ;
#15089 = CARTESIAN_POINT ( 'NONE',  ( 6.486361464680296507, 49.78306097819143616, 78.52964612251847143 ) ) ;
#15090 = ORIENTED_EDGE ( 'NONE', *, *, #873, .F. ) ;
#15091 = CARTESIAN_POINT ( 'NONE',  ( 5.384092268968043271, 50.76532863195453160, 75.97198585835440099 ) ) ;
#15092 = ADVANCED_FACE ( 'NONE', ( #14292 ), #7910, .T. ) ;
#15093 = CARTESIAN_POINT ( 'NONE',  ( 7.933465412281296203, 40.95200839197739384, 75.44378286633819641 ) ) ;
#15094 = CARTESIAN_POINT ( 'NONE',  ( 0.5221537403065010796, 44.16218137147969003, 45.55433879953098852 ) ) ;
#15096 = EDGE_CURVE ( 'NONE', #54, #10557, #16005, .T. ) ;
#15095 = CARTESIAN_POINT ( 'NONE',  ( -3.012418977206551052, 51.56146524693782141, 78.90943149866365047 ) ) ;
#15097 = CARTESIAN_POINT ( 'NONE',  ( -5.368445182934982185, 36.96218137147968008, 45.55433879953098852 ) ) ;
#15098 = CARTESIAN_POINT ( 'NONE',  ( 0.2541436421823711211, 38.02374091943176637, 92.79808879782399345 ) ) ;
#15099 = CARTESIAN_POINT ( 'NONE',  ( 0.7990284332011086121, 52.35254253780928480, 77.48826545068648386 ) ) ;
#15100 = CARTESIAN_POINT ( 'NONE',  ( 27.63948732994508006, 36.35905713404685713, 76.90433879953101837 ) ) ;
#15101 = CARTESIAN_POINT ( 'NONE',  ( 4.634072907867718527, 52.06528692560263494, 75.88092117868445996 ) ) ;
#15102 = EDGE_CURVE ( 'NONE', #14794, #17396, #14342, .T. ) ;
#15103 = CARTESIAN_POINT ( 'NONE',  ( 5.564133502460520297, 36.94922329332227662, 77.75193993234761081 ) ) ;
#15104 = CARTESIAN_POINT ( 'NONE',  ( -2.416137431568557314, 39.07291177436112406, 92.36746380123797451 ) ) ;
#15105 = EDGE_CURVE ( 'NONE', #7082, #3641, #20816, .T. ) ;
#15106 = DIRECTION ( 'NONE',  ( -0.5954989751681698529, 0.8033560671169786005, 5.234922652618076394E-17 ) ) ;
#15107 = ORIENTED_EDGE ( 'NONE', *, *, #4564, .F. ) ;
#15108 = CARTESIAN_POINT ( 'NONE',  ( 0.5596655318826941894, 52.96576883007725911, 75.97250646058495249 ) ) ;
#15109 = EDGE_CURVE ( 'NONE', #3380, #4927, #4807, .T. ) ;
#15110 = CARTESIAN_POINT ( 'NONE',  ( 0.3821786226492928651, 35.36301154328572949, 78.57639762306027365 ) ) ;
#15111 = LINE ( 'NONE', #13608, #13981 ) ;
#15112 = CARTESIAN_POINT ( 'NONE',  ( -4.505166693174837533, 37.68988179988254217, 78.83844719616611485 ) ) ;
#15113 = CARTESIAN_POINT ( 'NONE',  ( -5.154188915835984375, 42.64120994080404614, 92.36746380123797451 ) ) ;
#15114 = CARTESIAN_POINT ( 'NONE',  ( -5.087398782055174706, 37.36531724819641909, 77.33565342272370913 ) ) ;
#15115 = DIRECTION ( 'NONE',  ( -1.540237394707284220E-16, -1.793354297423764243E-16, 1.000000000000000000 ) ) ;
#15116 = DIRECTION ( 'NONE',  ( 0.8660254037844351549, -1.033702705553087164E-16, -0.5000000000000061062 ) ) ;
#15117 = ORIENTED_EDGE ( 'NONE', *, *, #4294, .F. ) ;
#15118 = VERTEX_POINT ( 'NONE', #3225 ) ;
#15119 = CARTESIAN_POINT ( 'NONE',  ( 8.243324203357053293, 41.86390813689740753, 79.54154676390322720 ) ) ;
#15120 = CYLINDRICAL_SURFACE ( 'NONE', #16571, 4.000000000000000000 ) ;
#15121 = CARTESIAN_POINT ( 'NONE',  ( 8.787829143201870252, 41.13140593384865440, 77.14698585835439815 ) ) ;
#15122 = EDGE_LOOP ( 'NONE', ( #15538, #2393, #18911, #3629 ) ) ;
#15123 = CARTESIAN_POINT ( 'NONE',  ( 0.4151831860546061348, 52.36151757739148849, 76.98461824414090415 ) ) ;
#15124 = CARTESIAN_POINT ( 'NONE',  ( 5.599231707071657738, 51.35236299959863970, 78.30875056423674607 ) ) ;
#15125 = LINE ( 'NONE', #535, #9209 ) ;
#15126 = CARTESIAN_POINT ( 'NONE',  ( -4.500660556396669065, 42.81632233694663370, 90.57058880294496817 ) ) ;
#15127 = EDGE_CURVE ( 'NONE', #20811, #10206, #10050, .T. ) ;
#15128 = CARTESIAN_POINT ( 'NONE',  ( -7.219979407079431866, 41.47817498120593882, 78.85792113001433279 ) ) ;
#15129 = CARTESIAN_POINT ( 'NONE',  ( 1.352400422481993658, 50.46853102219002096, 90.72683880123797451 ) ) ;
#15130 = B_SPLINE_CURVE_WITH_KNOTS ( 'NONE', 3,
 ( #6690, #3199, #16180, #16494, #107, #16395, #1821, #18087, #306, #8090, #12987, #16284, #11717, #19464, #8304, #17871, #16597, #1713, #4985 ),
 .UNSPECIFIED., .F., .F.,
 ( 4, 1, 1, 1, 1, 1, 1, 1, 1, 1, 1, 1, 1, 1, 1, 1, 4 ),
 ( 0.000000000000000000, 0.09472651553281030701, 0.1809448578637775085, 0.2575849355004761199, 0.3257111939256314703, 0.3842597268839244573, 0.4332657528852557616, 0.4727039292014991179, 0.5037345896081361074, 0.5551104982754543338, 0.6060435029138766527, 0.6590687186606726256, 0.7172582036121251114, 0.7797016678215834551, 0.8463570695623257034, 0.9189979831805518140, 1.000000000000000000 ),
 .UNSPECIFIED. ) ;
#15131 = UNCERTAINTY_MEASURE_WITH_UNIT (LENGTH_MEASURE( 1.000000000000000082E-05 ), #93, 'distance_accuracy_value', 'NONE');
#15132 = CARTESIAN_POINT ( 'NONE',  ( -4.477846259693478714, 37.66295064777091994, 53.55433879953098852 ) ) ;
#15133 = ORIENTED_EDGE ( 'NONE', *, *, #20137, .F. ) ;
#15134 = DIRECTION ( 'NONE',  ( 1.000000000000000000, 1.402518428993831183E-16, 1.213361030872721283E-32 ) ) ;
#15135 = ORIENTED_EDGE ( 'NONE', *, *, #10732, .T. ) ;
#15136 = CARTESIAN_POINT ( 'NONE',  ( 24.43948732994508077, 45.16218137147969003, 76.90433879953101837 ) ) ;
#15137 = CARTESIAN_POINT ( 'NONE',  ( -4.567115856812060670, 47.10047254335474065, 92.05496380123798872 ) ) ;
#15138 =( BOUNDED_CURVE ( )  B_SPLINE_CURVE ( 2, ( #4009, #8925, #10530, #15414, #13487, #828, #7315, #19958, #5388 ),
 .UNSPECIFIED., .F., .F. ) 
 B_SPLINE_CURVE_WITH_KNOTS ( ( 3, 2, 2, 2, 3 ),
 ( 0.5133706321031978881, 0.5208165472167179955, 0.5468573745775568984, 0.5728982019383959123, 0.5936396777664850744 ),
 .UNSPECIFIED. ) 
 CURVE ( )  GEOMETRIC_REPRESENTATION_ITEM ( )  RATIONAL_B_SPLINE_CURVE ( ( 0.9689162004489071389, 0.9782346954085345825, 1.000000000000000000, 0.9238795325112867385, 1.000000000000000000, 0.9238795325112867385, 1.000000000000000000, 0.9393701738211922558, 0.9753234597473514622 ) ) 
 REPRESENTATION_ITEM ( '' )  );
#15139 = ORIENTED_EDGE ( 'NONE', *, *, #15893, .F. ) ;
#15140 = FACE_OUTER_BOUND ( 'NONE', #7659, .T. ) ;
#15141 = CARTESIAN_POINT ( 'NONE',  ( -2.952897068019848525, 51.57503392883338478, 78.68920376838389075 ) ) ;
#15142 = LINE ( 'NONE', #2261, #16242 ) ;
#15143 = CARTESIAN_POINT ( 'NONE',  ( 5.349358414356570002, 50.78229839341420160, 77.28795170149270177 ) ) ;
#15144 = CARTESIAN_POINT ( 'NONE',  ( 0.5886303079273511596, 52.96555489546793183, 78.93669174070734584 ) ) ;
#15145 = VERTEX_POINT ( 'NONE', #2158 ) ;
#15146 = DIRECTION ( 'NONE',  ( -1.000000000000000000, -1.402518428993831676E-16, -1.196361017915039239E-16 ) ) ;
#15147 = ORIENTED_EDGE ( 'NONE', *, *, #17153, .F. ) ;
#15148 = LINE ( 'NONE', #11964, #16559 ) ;
#15149 = CARTESIAN_POINT ( 'NONE',  ( -5.368445182934982185, 36.96218137147968008, 93.55433879953098142 ) ) ;
#15150 = CARTESIAN_POINT ( 'NONE',  ( 5.359863228392665491, 37.54119487609694517, 75.97600981932362174 ) ) ;
#15151 = CARTESIAN_POINT ( 'NONE',  ( 3.722852957781953798, 40.32059543431686421, 95.05433879953096721 ) ) ;
#15152 = CARTESIAN_POINT ( 'NONE',  ( -4.007890887056448470, 40.01116025973682611, 91.54808879782400766 ) ) ;
#15153 = CARTESIAN_POINT ( 'NONE',  ( 5.544276951911416340, 50.64433212932689088, 78.27786821129558348 ) ) ;
#15154 = ORIENTED_EDGE ( 'NONE', *, *, #7235, .F. ) ;
#15155 = CARTESIAN_POINT ( 'NONE',  ( 8.797946357469053069, 41.16172786683149099, 78.83414475571305502 ) ) ;
#15156 = EDGE_CURVE ( 'NONE', #18045, #11193, #18218, .T. ) ;
#15157 = ORIENTED_EDGE ( 'NONE', *, *, #14197, .F. ) ;
#15158 = PLANE ( 'NONE',  #19693 ) ;
#15159 = CARTESIAN_POINT ( 'NONE',  ( 1.256812508749381774, 49.74246873332880625, 96.11746379953099506 ) ) ;
#15160 = CARTESIAN_POINT ( 'NONE',  ( 6.102441102155617969, 43.42752260303680600, 93.30496379953098085 ) ) ;
#15161 = PRODUCT_DEFINITION_SHAPE ( 'NONE', 'NONE',  #8857 ) ;
#15162 = CARTESIAN_POINT ( 'NONE',  ( -7.880650121838598032, 41.52863557963361529, 77.91116350996777840 ) ) ;
#15163 = ORIENTED_EDGE ( 'NONE', *, *, #9247, .T. ) ;
#15164 = FACE_OUTER_BOUND ( 'NONE', #338, .T. ) ;
#15165 = FACE_OUTER_BOUND ( 'NONE', #15871, .T. ) ;
#15166 = PLANE ( 'NONE',  #3166 ) ;
#15167 = ORIENTED_EDGE ( 'NONE', *, *, #2841, .T. ) ;
#15168 = CARTESIAN_POINT ( 'NONE',  ( 2.070819430837580022, 52.21461655967870996, 78.80944668400142916 ) ) ;
#15169 = VERTEX_POINT ( 'NONE', #20117 ) ;
#15170 = CARTESIAN_POINT ( 'NONE',  ( -4.802822372555619168, 51.17292061857877172, 76.30694920102484957 ) ) ;
#15171 = LINE ( 'NONE', #10729, #9527 ) ;
#15172 = CIRCLE ( 'NONE', #16192, 0.5999999999999928724 ) ;
#15173 = DIRECTION ( 'NONE',  ( 0.000000000000000000, 0.000000000000000000, 1.000000000000000000 ) ) ;
#15174 = CARTESIAN_POINT ( 'NONE',  ( -3.554968601118877469, 36.23337280359183410, 78.17158301229430606 ) ) ;
#15175 = CARTESIAN_POINT ( 'NONE',  ( 1.630627053521186864, 49.16218137147969003, 94.24615272619178086 ) ) ;
#15176 = CARTESIAN_POINT ( 'NONE',  ( -3.245728885430589017, 36.87898507402727688, 79.07903280936416479 ) ) ;
#15177 = ORIENTED_EDGE ( 'NONE', *, *, #15609, .F. ) ;
#15178 = ORIENTED_EDGE ( 'NONE', *, *, #20150, .F. ) ;
#15179 = EDGE_CURVE ( 'NONE', #19082, #8044, #7032, .T. ) ;
#15180 = CARTESIAN_POINT ( 'NONE',  ( 4.394267649348433835, 36.11327998621098345, 76.69403369658814995 ) ) ;
#15181 = ORIENTED_EDGE ( 'NONE', *, *, #30, .T. ) ;
#15182 = CARTESIAN_POINT ( 'NONE',  ( -0.9234155522616860345, 52.23375968936932168, 78.59964918550147672 ) ) ;
#15183 = DIRECTION ( 'NONE',  ( -0.4999999999999977240, 0.8660254037844398178, 0.000000000000000000 ) ) ;
#15184 = CARTESIAN_POINT ( 'NONE',  ( 5.611423337425062385, 41.22389019960463230, 94.08621380123797451 ) ) ;
#15185 = CARTESIAN_POINT ( 'NONE',  ( -3.364492789658395377, 52.20069827791003547, 76.33204918460485544 ) ) ;
#15186 = ORIENTED_EDGE ( 'NONE', *, *, #10821, .F. ) ;
#15187 = VERTEX_POINT ( 'NONE', #5553 ) ;
#15188 = CIRCLE ( 'NONE', #11131, 8.199999999999995737 ) ;
#15189 = CARTESIAN_POINT ( 'NONE',  ( 6.761793986577667503, 50.49362507459272820, 79.13556070921569585 ) ) ;
#15190 = ORIENTED_EDGE ( 'NONE', *, *, #10100, .T. ) ;
#15191 = DIRECTION ( 'NONE',  ( -1.779391786395883536E-16, -5.922860397471805611E-17, 1.000000000000000000 ) ) ;
#15192 = CARTESIAN_POINT ( 'NONE',  ( 5.991756872021341884, 37.25478729691962343, 75.38041148603002739 ) ) ;
#15193 = CARTESIAN_POINT ( 'NONE',  ( 8.572560397843592028, 40.48623184761532912, 75.53366564255911442 ) ) ;
#15194 = ADVANCED_FACE ( 'NONE', ( #11642 ), #233, .T. ) ;
#15195 = DIRECTION ( 'NONE',  ( -0.000000000000000000, -0.000000000000000000, 1.000000000000000000 ) ) ;
#15196 = CARTESIAN_POINT ( 'NONE',  ( 4.539372959821318609, 52.13523796247791608, 76.58963291717793709 ) ) ;
#15197 = LINE ( 'NONE', #8290, #2471 ) ;
#15198 = CARTESIAN_POINT ( 'NONE',  ( -5.154188915835984375, 42.64120994080404614, 96.11746380123797451 ) ) ;
#15199 = LINE ( 'NONE', #14512, #9787 ) ;
#15200 = CARTESIAN_POINT ( 'NONE',  ( 2.916646314870772194, 38.79555996194921619, 92.55433879953098142 ) ) ;
#15201 = CARTESIAN_POINT ( 'NONE',  ( -0.4699484075729998267, 52.36218137147968577, 87.21440135111343750 ) ) ;
#15202 = CARTESIAN_POINT ( 'NONE',  ( -5.784195910403845176, 44.99242805365518194, 93.38308880123798872 ) ) ;
#15203 = CIRCLE ( 'NONE', #7394, 5.199999999999999289 ) ;
#15204 = CARTESIAN_POINT ( 'NONE',  ( 8.362028646804796850, 41.75872088733057552, 76.06672873082523267 ) ) ;
#15205 = VERTEX_POINT ( 'NONE', #3540 ) ;
#15206 = EDGE_CURVE ( 'NONE', #14920, #13884, #4923, .T. ) ;
#15207 = CARTESIAN_POINT ( 'NONE',  ( 0.4810581700086011270, 52.35504993940188001, 75.98243536310876323 ) ) ;
#15208 = EDGE_CURVE ( 'NONE', #5035, #6017, #1850, .T. ) ;
#15209 = EDGE_CURVE ( 'NONE', #20066, #2125, #10260, .T. ) ;
#15210 = VERTEX_POINT ( 'NONE', #12058 ) ;
#15211 = CARTESIAN_POINT ( 'NONE',  ( 24.43948732994508788, 45.16218137147969003, 74.70433879953100131 ) ) ;
#15212 = CARTESIAN_POINT ( 'NONE',  ( 9.271561067608034890, 45.68041113525027441, 79.47125056423675460 ) ) ;
#15213 = CARTESIAN_POINT ( 'NONE',  ( -2.055347584452832166, 51.31805217249780782, 75.45433879953087342 ) ) ;
#15214 = CARTESIAN_POINT ( 'NONE',  ( -5.784195910403845176, 44.99242805365518194, 94.78933880123798872 ) ) ;
#15215 = VECTOR ( 'NONE', #9276, 1000.000000000000000 ) ;
#15216 = DIRECTION ( 'NONE',  ( 1.193617070626243484E-16, 1.000000000000000000, 0.000000000000000000 ) ) ;
#15217 = FACE_OUTER_BOUND ( 'NONE', #5411, .T. ) ;
#15218 = LINE ( 'NONE', #629, #12649 ) ;
#15219 = EDGE_CURVE ( 'NONE', #9753, #3490, #7141, .T. ) ;
#15220 = DIRECTION ( 'NONE',  ( -0.9485903129789529098, 0.3165065846431826535, -8.934458285744997376E-17 ) ) ;
#15221 = ORIENTED_EDGE ( 'NONE', *, *, #6778, .F. ) ;
#15222 = CIRCLE ( 'NONE', #14193, 8.199999999999995737 ) ;
#15223 = CARTESIAN_POINT ( 'NONE',  ( 9.177137044501376906, 42.29818641127601353, 79.38025142445083304 ) ) ;
#15224 = LINE ( 'NONE', #5534, #6349 ) ;
#15225 = CARTESIAN_POINT ( 'NONE',  ( 0.6324608792002816005, 52.96167523169288671, 75.97329777450663357 ) ) ;
#15226 = VERTEX_POINT ( 'NONE', #10369 ) ;
#15227 = CARTESIAN_POINT ( 'NONE',  ( 0.4849271306368859724, 52.36220339060425033, 78.92934173667400444 ) ) ;
#15228 = LINE ( 'NONE', #10564, #9103 ) ;
#15229 = CARTESIAN_POINT ( 'NONE',  ( -0.3594811632358396736, 49.16218137147969003, 92.76483168766085896 ) ) ;
#15230 = CARTESIAN_POINT ( 'NONE',  ( -2.077846259693550746, 39.65884927180063357, 90.72683880294498238 ) ) ;
#15231 = VECTOR ( 'NONE', #18524, 1000.000000000000000 ) ;
#15232 = CARTESIAN_POINT ( 'NONE',  ( -7.787617544678308690, 41.24164596078931311, 78.75487387812985673 ) ) ;
#15233 = CARTESIAN_POINT ( 'NONE',  ( -3.188853836583637413, 36.87695358026009274, 77.96849812480175501 ) ) ;
#15234 = CARTESIAN_POINT ( 'NONE',  ( 1.352400422481993658, 50.46853102219002096, 93.07058880123798872 ) ) ;
#15235 = CARTESIAN_POINT ( 'NONE',  ( 6.882613847952937292, 37.89136107556471700, 76.65924029158320252 ) ) ;
#15236 = ORIENTED_EDGE ( 'NONE', *, *, #10136, .T. ) ;
#15237 = EDGE_CURVE ( 'NONE', #20138, #7199, #16077, .T. ) ;
#15238 = CARTESIAN_POINT ( 'NONE',  ( -1.493738069816088920, 38.45421922485636657, 72.45433879953085921 ) ) ;
#15239 = ORIENTED_EDGE ( 'NONE', *, *, #7548, .T. ) ;
#15240 = DIRECTION ( 'NONE',  ( -1.540237394707283727E-16, -1.793354297423763257E-16, 1.000000000000000000 ) ) ;
#15241 = EDGE_CURVE ( 'NONE', #13048, #8338, #18430, .T. ) ;
#15242 = CARTESIAN_POINT ( 'NONE',  ( 1.352400422481993658, 50.46853102219002096, 91.82058880123801714 ) ) ;
#15243 = ORIENTED_EDGE ( 'NONE', *, *, #14856, .F. ) ;
#15244 = CARTESIAN_POINT ( 'NONE',  ( 8.443422548343662015, 42.04239353520513589, 78.13669174070733447 ) ) ;
#15245 = AXIS2_PLACEMENT_3D ( 'NONE', #17265, #16949, #4177 ) ;
#15246 = EDGE_CURVE ( 'NONE', #4372, #9222, #5439, .T. ) ;
#15247 = LINE ( 'NONE', #7142, #13209 ) ;
#15248 = CARTESIAN_POINT ( 'NONE',  ( -3.850375455727051310, 51.85350431403718119, 79.38294305353919356 ) ) ;
#15249 = DIRECTION ( 'NONE',  ( 0.000000000000000000, 0.000000000000000000, -1.000000000000000000 ) ) ;
#15250 = CARTESIAN_POINT ( 'NONE',  ( 0.8456369902943451367, 52.35216224083615089, 76.46781884397893236 ) ) ;
#15251 = CARTESIAN_POINT ( 'NONE',  ( 0.3352349842281855952, 52.35619972255046406, 78.67509294885779525 ) ) ;
#15252 = VERTEX_POINT ( 'NONE', #16839 ) ;
#15253 = CARTESIAN_POINT ( 'NONE',  ( 8.300594306733913186, 41.56682737740558764, 77.52492703482499792 ) ) ;
#15254 = ORIENTED_EDGE ( 'NONE', *, *, #2874, .T. ) ;
#15255 = DIRECTION ( 'NONE',  ( -1.193617070626243484E-16, -1.000000000000000000, -0.000000000000000000 ) ) ;
#15256 = CARTESIAN_POINT ( 'NONE',  ( 6.960009239587057195, 50.34721145179211987, 76.80946857459053945 ) ) ;
#15257 = LINE ( 'NONE', #15468, #13928 ) ;
#15258 = CARTESIAN_POINT ( 'NONE',  ( -7.407177866501955421, 40.34522932431062969, 77.72181725404989550 ) ) ;
#15259 = CARTESIAN_POINT ( 'NONE',  ( 4.673174852049362116, 39.63213674411673537, 93.11058879782397923 ) ) ;
#15260 = CARTESIAN_POINT ( 'NONE',  ( -4.716387082485073989, 37.09126585098686490, 75.36022115247205022 ) ) ;
#15261 = AXIS2_PLACEMENT_3D ( 'NONE', #14689, #6487, #17778 ) ;
#15262 = ORIENTED_EDGE ( 'NONE', *, *, #14814, .F. ) ;
#15263 = FACE_BOUND ( 'NONE', #20967, .T. ) ;
#15264 =( BOUNDED_CURVE ( )  B_SPLINE_CURVE ( 3, ( #8438, #39, #9833, #11645 ),
 .UNSPECIFIED., .F., .F. ) 
 B_SPLINE_CURVE_WITH_KNOTS ( ( 4, 4 ),
 ( 1.982313172862385731, 2.094395102393195263 ),
 .UNSPECIFIED. ) 
 CURVE ( )  GEOMETRIC_REPRESENTATION_ITEM ( )  RATIONAL_B_SPLINE_CURVE ( ( 1.000000000000000000, 0.9989534107080366709, 0.9989534107080366709, 1.000000000000000000 ) ) 
 REPRESENTATION_ITEM ( '' )  );
#15265 = EDGE_LOOP ( 'NONE', ( #2277, #10686, #11611, #14958 ) ) ;
#15266 = CARTESIAN_POINT ( 'NONE',  ( -3.872072204604002810, 50.91822502938001094, 75.38014013087713749 ) ) ;
#15267 = EDGE_CURVE ( 'NONE', #11453, #1174, #3431, .T. ) ;
#15268 = CARTESIAN_POINT ( 'NONE',  ( 4.987494971863720927, 47.58855820898865829, 93.46121379953098085 ) ) ;
#15269 = CARTESIAN_POINT ( 'NONE',  ( 1.868012774839550749, 39.13936707477651566, 93.07058879953099506 ) ) ;
#15270 = VERTEX_POINT ( 'NONE', #13334 ) ;
#15271 = CARTESIAN_POINT ( 'NONE',  ( -7.611372734017124664, 43.12018948500615778, 75.45433879953087342 ) ) ;
#15272 = ORIENTED_EDGE ( 'NONE', *, *, #12249, .F. ) ;
#15273 = DIRECTION ( 'NONE',  ( 1.540237394707284220E-16, 1.793354297423764243E-16, -1.000000000000000000 ) ) ;
#15274 = CARTESIAN_POINT ( 'NONE',  ( -7.077609990433002096, 44.22210830145579763, 72.45432679953087529 ) ) ;
#15275 = B_SPLINE_CURVE_WITH_KNOTS ( 'NONE', 3,
 ( #16727, #2469, #542, #20435, #7244, #16832, #17145, #5429, #12051, #650, #18422, #7022, #11836, #18309, #13839, #5546 ),
 .UNSPECIFIED., .F., .F.,
 ( 4, 2, 2, 2, 2, 2, 2, 4 ),
 ( 0.000000000000000000, 0.0002723625545810964919, 0.0005447251091621929837, 0.001089450218324406784, 0.001361812772905513684, 0.001634175327486620368, 0.001906537882067727485, 0.002178900436648834385 ),
 .UNSPECIFIED. ) ;
#15276 = ORIENTED_EDGE ( 'NONE', *, *, #12314, .F. ) ;
#15277 = LINE ( 'NONE', #2512, #20026 ) ;
#15278 = AXIS2_PLACEMENT_3D ( 'NONE', #14082, #15894, #6087 ) ;
#15279 = CARTESIAN_POINT ( 'NONE',  ( -3.350035803220276609, 49.20851703305431357, 93.38308880123798872 ) ) ;
#15280 = VERTEX_POINT ( 'NONE', #13644 ) ;
#15281 = CARTESIAN_POINT ( 'NONE',  ( -4.445462123736771076, 50.68136173637071096, 76.24916814194597237 ) ) ;
#15282 = DIRECTION ( 'NONE',  ( -1.540237394707284220E-16, -1.793354297423764243E-16, 1.000000000000000000 ) ) ;
#15283 = VECTOR ( 'NONE', #15845, 1000.000000000000114 ) ;
#15284 = CARTESIAN_POINT ( 'NONE',  ( -4.894326847483571719, 37.22270278754029960, 76.26481528174605273 ) ) ;
#15285 = CIRCLE ( 'NONE', #6796, 0.9921021478795063464 ) ;
#15286 = CARTESIAN_POINT ( 'NONE',  ( 28.52215374030649642, 44.16218137147969003, 105.5543387995310098 ) ) ;
#15287 = AXIS2_PLACEMENT_3D ( 'NONE', #12242, #19118, #19312 ) ;
#15288 = DIRECTION ( 'NONE',  ( -0.3165065846431827090, -0.9485903129789527988, 0.000000000000000000 ) ) ;
#15289 = EDGE_CURVE ( 'NONE', #16499, #10028, #8333, .T. ) ;
#15290 = VERTEX_POINT ( 'NONE', #6720 ) ;
#15291 = EDGE_LOOP ( 'NONE', ( #4357, #17162, #13754 ) ) ;
#15292 = CARTESIAN_POINT ( 'NONE',  ( 2.032153066220215631, 52.20217092279865767, 76.00457246026148539 ) ) ;
#15293 = AXIS2_PLACEMENT_3D ( 'NONE', #10828, #15709, #16016 ) ;
#15294 = AXIS2_PLACEMENT_3D ( 'NONE', #8039, #19519, #14526 ) ;
#15295 = ORIENTED_EDGE ( 'NONE', *, *, #1014, .T. ) ;
#15296 = CARTESIAN_POINT ( 'NONE',  ( 31.22215374030650281, 42.76218137147968434, 78.80433879953099563 ) ) ;
#15297 = CARTESIAN_POINT ( 'NONE',  ( 11.22215374030650281, 51.36218137147968577, 64.80574467885102763 ) ) ;
#15298 = CARTESIAN_POINT ( 'NONE',  ( -7.210081352984018643, 41.43222958516458476, 78.77893318671775091 ) ) ;
#15299 = ORIENTED_EDGE ( 'NONE', *, *, #4557, .T. ) ;
#15300 = EDGE_LOOP ( 'NONE', ( #14302, #2081, #18061, #5359 ) ) ;
#15301 = VECTOR ( 'NONE', #3438, 1000.000000000000000 ) ;
#15302 = CARTESIAN_POINT ( 'NONE',  ( -5.955451856753747997, 38.00651308716548726, 78.18375056423674607 ) ) ;
#15303 = ORIENTED_EDGE ( 'NONE', *, *, #18103, .T. ) ;
#15304 = DIRECTION ( 'NONE',  ( -1.110223024625156540E-16, -1.000000000000000000, -5.922860397471808077E-17 ) ) ;
#15305 = CARTESIAN_POINT ( 'NONE',  ( 2.119851040271390374, 52.81592988514039178, 76.48963291717792856 ) ) ;
#15306 = DIRECTION ( 'NONE',  ( 1.000000000000000000, 1.402518428993831183E-16, -4.865963288531423895E-32 ) ) ;
#15307 = DIRECTION ( 'NONE',  ( 0.3165065846431826535, 0.9485903129789529098, 2.188653791613874008E-16 ) ) ;
#15308 = CARTESIAN_POINT ( 'NONE',  ( 0.5221537403065009686, 44.16218137147968292, 79.40903933791013003 ) ) ;
#15309 = CARTESIAN_POINT ( 'NONE',  ( -1.477846259693495146, 47.62628298661744708, 58.55433879953100984 ) ) ;
#15310 = AXIS2_PLACEMENT_3D ( 'NONE', #6896, #18499, #11804 ) ;
#15311 = CARTESIAN_POINT ( 'NONE',  ( 0.7823402848519026564, 52.35267412999201042, 77.46299673659909502 ) ) ;
#15312 = EDGE_CURVE ( 'NONE', #5547, #4359, #5620, .T. ) ;
#15313 = VECTOR ( 'NONE', #15777, 1000.000000000000000 ) ;
#15314 = PLANE ( 'NONE',  #7125 ) ;
#15315 = CARTESIAN_POINT ( 'NONE',  ( 4.290864208700578608, 51.39396841940111926, 75.72008365543779007 ) ) ;
#15316 = CARTESIAN_POINT ( 'NONE',  ( 5.025485839985549319, 41.56218137147963887, 92.28933880294496817 ) ) ;
#15317 = VECTOR ( 'NONE', #4044, 1000.000000000000000 ) ;
#15318 = CARTESIAN_POINT ( 'NONE',  ( -7.948766803159697858, 41.75119145221206196, 78.75998376317852490 ) ) ;
#15319 = ORIENTED_EDGE ( 'NONE', *, *, #8479, .F. ) ;
#15320 = PLANE ( 'NONE',  #11201 ) ;
#15321 = B_SPLINE_CURVE_WITH_KNOTS ( 'NONE', 3,
 ( #6329, #19009, #20692, #16142, #17518, #11257, #17727, #3159 ),
 .UNSPECIFIED., .F., .F.,
 ( 4, 2, 2, 4 ),
 ( 0.000000000000000000, 0.0002990901329414861185, 0.0004486351994122288796, 0.0005981802658829716950 ),
 .UNSPECIFIED. ) ;
#15322 = ORIENTED_EDGE ( 'NONE', *, *, #16747, .F. ) ;
#15323 = DIRECTION ( 'NONE',  ( 1.084202172485505420E-16, 1.000000000000000000, 0.000000000000000000 ) ) ;
#15324 = EDGE_CURVE ( 'NONE', #14379, #6954, #11744, .T. ) ;
#15325 = DIRECTION ( 'NONE',  ( 0.000000000000000000, 0.000000000000000000, -1.000000000000000000 ) ) ;
#15326 = FACE_OUTER_BOUND ( 'NONE', #13431, .T. ) ;
#15327 = CARTESIAN_POINT ( 'NONE',  ( 3.460444912181559474, 49.25145096859824889, 95.64871380123798872 ) ) ;
#15328 = CARTESIAN_POINT ( 'NONE',  ( -4.603341302083753028, 37.00776348676620842, 77.20593245741272881 ) ) ;
#15329 = CARTESIAN_POINT ( 'NONE',  ( 0.5221537403065096283, 50.16218137147969713, 59.55433879953099563 ) ) ;
#15330 = CARTESIAN_POINT ( 'NONE',  ( 1.087740465381641375, 52.94398708878058102, 76.77198585835439815 ) ) ;
#15331 = CARTESIAN_POINT ( 'NONE',  ( 5.847431522242757751, 51.16902779423016767, 77.98758453411963387 ) ) ;
#15332 = ORIENTED_EDGE ( 'NONE', *, *, #10784, .T. ) ;
#15333 = CARTESIAN_POINT ( 'NONE',  ( 8.913594855155908547, 41.50833375100289402, 79.54698768757486960 ) ) ;
#15334 = LINE ( 'NONE', #18620, #7015 ) ;
#15335 = CARTESIAN_POINT ( 'NONE',  ( 8.951594291416542504, 41.62222047211530906, 76.36070165242202279 ) ) ;
#15336 = DIRECTION ( 'NONE',  ( 1.000000000000000000, 0.000000000000000000, 0.000000000000000000 ) ) ;
#15337 = CARTESIAN_POINT ( 'NONE',  ( -1.477846259693488706, 49.81903562097206617, 123.5543387995310098 ) ) ;
#15338 = CARTESIAN_POINT ( 'NONE',  ( 5.631785411401764918, 36.99756487055721976, 77.76022115247205591 ) ) ;
#15339 = LINE ( 'NONE', #5540, #15231 ) ;
#15340 = VECTOR ( 'NONE', #8650, 1000.000000000000000 ) ;
#15341 = CARTESIAN_POINT ( 'NONE',  ( 2.421193248165596668, 49.85372324935340060, 82.45433879953087342 ) ) ;
#15342 = CARTESIAN_POINT ( 'NONE',  ( -7.088838830337594210, 47.02440864255881081, 77.61879955032603107 ) ) ;
#15343 = CARTESIAN_POINT ( 'NONE',  ( 5.611423337425062385, 41.22389019960463230, 90.33621380123798872 ) ) ;
#15344 = B_SPLINE_SURFACE_WITH_KNOTS ( 'NONE', 3, 1, ( 
 ( #12514, #18996 ),
 ( #7722, #4413 ),
 ( #11034, #6115 ),
 ( #17403, #2830 ),
 ( #2928, #1231 ),
 ( #14204, #12620 ),
 ( #17504, #16025 ),
 ( #8245, #19300 ),
 ( #16129, #4827 ),
 ( #1547, #6221 ),
 ( #16334, #19198 ),
 ( #6316, #4613 ),
 ( #53, #7828 ),
 ( #8033, #13040 ),
 ( #12720, #14732 ),
 ( #4714, #154 ),
 ( #11135, #20986 ),
 ( #1443, #3245 ),
 ( #14520, #6420 ) ),
 .UNSPECIFIED., .F., .F., .F.,
 ( 4, 1, 1, 1, 1, 1, 1, 1, 1, 1, 1, 1, 1, 1, 1, 1, 4 ),
 ( 2, 2 ),
 ( 0.000000000000000000, 0.05434379794353864229, 0.1062390698768248820, 0.1553778989748225425, 0.2029887854916514467, 0.2486500052201169320, 0.2921085583616858661, 0.3352193261980264682, 0.3771870632897987852, 0.4223876994541358454, 0.4752030700363142346, 0.5373302487560115415, 0.6091097927081512431, 0.6911313100281405442, 0.7836801803933998167, 0.8864064767870927231, 1.000000000000000000 ),
 ( 0.000000000000000000, 1.000000000000000000 ),
 .UNSPECIFIED. ) ;
#15345 = CARTESIAN_POINT ( 'NONE',  ( 6.658811665516601863, 37.73144022991658630, 75.70392102816973079 ) ) ;
#15346 = ORIENTED_EDGE ( 'NONE', *, *, #11714, .F. ) ;
#15347 = CARTESIAN_POINT ( 'NONE',  ( 5.574007247060956516, 50.61635935010243514, 77.05868164888072158 ) ) ;
#15348 = ORIENTED_EDGE ( 'NONE', *, *, #18034, .T. ) ;
#15349 = AXIS2_PLACEMENT_3D ( 'NONE', #13219, #9937, #19900 ) ;
#15350 = PLANE ( 'NONE',  #7132 ) ;
#15351 = VECTOR ( 'NONE', #8427, 1000.000000000000114 ) ;
#15352 = CARTESIAN_POINT ( 'NONE',  ( 3.460444912181559474, 49.25145096859824889, 92.99246380123798872 ) ) ;
#15353 = VERTEX_POINT ( 'NONE', #15561 ) ;
#15354 = CARTESIAN_POINT ( 'NONE',  ( 6.660594192354428955, 43.89417127335556046, 94.51683879782399345 ) ) ;
#15355 = CARTESIAN_POINT ( 'NONE',  ( 0.5221537403065076299, 49.16218137147969003, 94.29136871766880290 ) ) ;
#15356 = CARTESIAN_POINT ( 'NONE',  ( -3.355600405723123902, 52.20705244989922988, 78.36353918055804968 ) ) ;
#15357 = CARTESIAN_POINT ( 'NONE',  ( 30.92220646078100188, 45.56218137147968861, 62.80715055817104542 ) ) ;
#15358 = DIRECTION ( 'NONE',  ( -1.000000000000000000, 4.930380657631323784E-32, -3.893792155548169402E-16 ) ) ;
#15359 = FACE_OUTER_BOUND ( 'NONE', #4629, .T. ) ;
#15360 = VERTEX_POINT ( 'NONE', #6069 ) ;
#15361 = ADVANCED_FACE ( 'NONE', ( #2676, #769 ), #9292, .F. ) ;
#15362 = LINE ( 'NONE', #3958, #12903 ) ;
#15363 = ORIENTED_EDGE ( 'NONE', *, *, #10714, .T. ) ;
#15364 = DIRECTION ( 'NONE',  ( 1.779391786395883536E-16, 5.922860397471806844E-17, -1.000000000000000000 ) ) ;
#15365 = CARTESIAN_POINT ( 'NONE',  ( -0.4699484075729998822, 52.36218137147968577, 83.03825919817350609 ) ) ;
#15366 = EDGE_CURVE ( 'NONE', #11953, #18462, #14332, .T. ) ;
#15367 = PLANE ( 'NONE',  #20970 ) ;
#15368 = CARTESIAN_POINT ( 'NONE',  ( 6.030184373421643151, 51.03403562479821431, 79.53335372712579954 ) ) ;
#15369 = CARTESIAN_POINT ( 'NONE',  ( 6.522436035574397550, 49.75115376156129798, 75.45433879953087342 ) ) ;
#15370 = VECTOR ( 'NONE', #7939, 1000.000000000000114 ) ;
#15371 = CARTESIAN_POINT ( 'NONE',  ( 5.052198367669454626, 48.31320248322254685, 93.42308879782400766 ) ) ;
#15372 = CARTESIAN_POINT ( 'NONE',  ( 6.267060310175591731, 50.01365258206436692, 79.25094314227297332 ) ) ;
#15373 = ADVANCED_FACE ( 'NONE', ( #10890 ), #5970, .F. ) ;
#15374 = VECTOR ( 'NONE', #20412, 1000.000000000000000 ) ;
#15375 = ORIENTED_EDGE ( 'NONE', *, *, #4412, .T. ) ;
#15376 = CARTESIAN_POINT ( 'NONE',  ( 8.284287939682402069, 41.54251913719888734, 78.93613448519710118 ) ) ;
#15377 = EDGE_CURVE ( 'NONE', #496, #1879, #4167, .T. ) ;
#15378 = ORIENTED_EDGE ( 'NONE', *, *, #253, .F. ) ;
#15379 = CARTESIAN_POINT ( 'NONE',  ( -7.202537930885374529, 41.41097462079392955, 78.61536821129558916 ) ) ;
#15380 = CARTESIAN_POINT ( 'NONE',  ( 5.544968037009670780, 45.50804040601273925, 93.38308879953099506 ) ) ;
#15381 = CARTESIAN_POINT ( 'NONE',  ( -0.8237052942265477018, 49.18499566818285018, 91.19558879953099506 ) ) ;
#15382 = CARTESIAN_POINT ( 'NONE',  ( -7.208606195151301854, 41.85401949100505448, 77.76017221056694950 ) ) ;
#15383 = VERTEX_POINT ( 'NONE', #15455 ) ;
#15384 = CARTESIAN_POINT ( 'NONE',  ( -5.784195910403845176, 44.99242805365518194, 92.28933880123798872 ) ) ;
#15385 = CARTESIAN_POINT ( 'NONE',  ( 0.5021497504818818181, 52.96224978603238043, 77.38972049658568153 ) ) ;
#15387 = CARTESIAN_POINT ( 'NONE',  ( 5.632375035844972899, 36.99798619459680538, 75.36061873398452349 ) ) ;
#15386 = B_SPLINE_CURVE_WITH_KNOTS ( 'NONE', 3,
 ( #3905, #13394, #18383, #10213, #15095, #10428, #14987, #505, #8711, #7316, #6982, #18595, #2429, #13488 ),
 .UNSPECIFIED., .F., .F.,
 ( 4, 2, 2, 2, 2, 2, 4 ),
 ( 0.000000000000000000, 0.0006081318354814772235, 0.0009121977532222158352, 0.001216263670962954230, 0.001824395506444449885, 0.002128461424185192508, 0.002432527341925936649 ),
 .UNSPECIFIED. ) ;
#15388 = CARTESIAN_POINT ( 'NONE',  ( -4.804534436424639843, 51.17169724042062739, 78.47639829077699858 ) ) ;
#15389 = AXIS2_PLACEMENT_3D ( 'NONE', #8315, #12042, #2031 ) ;
#15390 = ORIENTED_EDGE ( 'NONE', *, *, #3889, .T. ) ;
#15391 = FACE_BOUND ( 'NONE', #6461, .T. ) ;
#15392 = CARTESIAN_POINT ( 'NONE',  ( 2.043125170982144745, 38.48583871533720213, 95.17996380123798872 ) ) ;
#15393 = ORIENTED_EDGE ( 'NONE', *, *, #17392, .T. ) ;
#15394 = CARTESIAN_POINT ( 'NONE',  ( -4.429725150862205751, 50.69260680101952232, 76.11505395997643575 ) ) ;
#15395 = CARTESIAN_POINT ( 'NONE',  ( -0.07555581626192670042, 50.25084051303456789, 85.06567965797613340 ) ) ;
#15396 = CARTESIAN_POINT ( 'NONE',  ( 5.611423337425062385, 41.22389019960463230, 91.42996380123798872 ) ) ;
#15397 = APPLICATION_PROTOCOL_DEFINITION ( 'draft international standard', 'automotive_design', 1998, #5588 ) ;
#15398 = CARTESIAN_POINT ( 'NONE',  ( 6.153536035488349043, 50.12267912296926653, 77.68963291717793140 ) ) ;
#15399 = ADVANCED_FACE ( 'NONE', ( #7356 ), #20327, .F. ) ;
#15400 = CARTESIAN_POINT ( 'NONE',  ( 0.4081407667913234394, 52.96145465813116004, 78.87521754079256198 ) ) ;
#15401 = CARTESIAN_POINT ( 'NONE',  ( -7.230623167723755351, 41.49097751518757349, 78.30226502014330947 ) ) ;
#15402 = ORIENTED_EDGE ( 'NONE', *, *, #21034, .T. ) ;
#15403 = ORIENTED_EDGE ( 'NONE', *, *, #810, .T. ) ;
#15404 = CARTESIAN_POINT ( 'NONE',  ( 2.078566409199763765, 52.20180493653207776, 76.15080458372598571 ) ) ;
#15405 = VERTEX_POINT ( 'NONE', #17154 ) ;
#15406 = LINE ( 'NONE', #5700, #14324 ) ;
#15407 = CARTESIAN_POINT ( 'NONE',  ( 6.198496396448986090, 45.68315280215533392, 94.24246380123798872 ) ) ;
#15408 = VERTEX_POINT ( 'NONE', #2574 ) ;
#15409 = CARTESIAN_POINT ( 'NONE',  ( -3.154801521863568325, 47.83913663364971569, 83.28180655319408743 ) ) ;
#15410 = ORIENTED_EDGE ( 'NONE', *, *, #9240, .T. ) ;
#15411 = CARTESIAN_POINT ( 'NONE',  ( 4.396638484636539168, 51.32665516437340614, 79.26957207196610966 ) ) ;
#15412 = CARTESIAN_POINT ( 'NONE',  ( 5.928963754087452465, 43.92611494815086814, 91.46996379953098710 ) ) ;
#15413 = AXIS2_PLACEMENT_3D ( 'NONE', #8286, #14767, #6673 ) ;
#15414 = CARTESIAN_POINT ( 'NONE',  ( 5.568489401881125289, 48.03437091500647682, 92.91433880123805977 ) ) ;
#15415 = CARTESIAN_POINT ( 'NONE',  ( 0.5221537403065015237, 44.16218137147968292, 75.45433879953088763 ) ) ;
#15416 = LINE ( 'NONE', #13914, #10653 ) ;
#15417 = CARTESIAN_POINT ( 'NONE',  ( 4.394343283833276992, 39.11584570990505938, 94.00808880123797451 ) ) ;
#15418 = CARTESIAN_POINT ( 'NONE',  ( 0.8140313835477279714, 52.35242423403212086, 77.51877209028926075 ) ) ;
#15419 = DIRECTION ( 'NONE',  ( -1.402518428993831183E-16, 1.000000000000000000, -3.469446951953617640E-16 ) ) ;
#15420 = DIRECTION ( 'NONE',  ( 0.8033560671169786005, 0.5954989751681698529, 2.305299702067830011E-16 ) ) ;
#15421 = CARTESIAN_POINT ( 'NONE',  ( -0.2125050281363792815, 38.58189400963055959, 92.05496380294498238 ) ) ;
#15422 = CARTESIAN_POINT ( 'NONE',  ( -4.348661956197086731, 37.56557963644259956, 78.93669174070734584 ) ) ;
#15423 = ORIENTED_EDGE ( 'NONE', *, *, #3745, .T. ) ;
#15424 = VERTEX_POINT ( 'NONE', #189 ) ;
#15425 = CARTESIAN_POINT ( 'NONE',  ( 4.199109002476567376, 47.83913663364971569, 95.05036078555451695 ) ) ;
#15426 = DIRECTION ( 'NONE',  ( -0.5941461771851693774, -0.8043570849667760481, -2.357623395011396791E-16 ) ) ;
#15427 = CARTESIAN_POINT ( 'NONE',  ( 2.522153740306506187, 49.81903562097208038, 77.15433879953100416 ) ) ;
#15428 = CARTESIAN_POINT ( 'NONE',  ( -0.3080929418689875576, 37.85583172076933778, 92.60183880123797451 ) ) ;
#15429 = EDGE_CURVE ( 'NONE', #17689, #20491, #20829, .T. ) ;
#15430 = CARTESIAN_POINT ( 'NONE',  ( -4.877877647307895970, 37.21055242598473001, 76.09452555557021469 ) ) ;
#15431 = CARTESIAN_POINT ( 'NONE',  ( -8.275363242949740794, 42.78218605590705437, 78.99227765976493743 ) ) ;
#15432 = CARTESIAN_POINT ( 'NONE',  ( 5.427780505986065762, 36.85179043424346190, 77.43080938776617472 ) ) ;
#15433 = CARTESIAN_POINT ( 'NONE',  ( -4.677846234369972045, 43.47758828951656795, 93.04575777171294249 ) ) ;
#15434 = VERTEX_POINT ( 'NONE', #17563 ) ;
#15435 = EDGE_LOOP ( 'NONE', ( #4688, #13312, #20464, #4696, #13694 ) ) ;
#15436 = CARTESIAN_POINT ( 'NONE',  ( 8.534545774096850224, 42.73671765915654674, 79.25343573416346032 ) ) ;
#15437 = CARTESIAN_POINT ( 'NONE',  ( 8.214799251806553571, 41.32260305165857517, 77.14698585835439815 ) ) ;
#15438 = LINE ( 'NONE', #10456, #12323 ) ;
#15439 = LINE ( 'NONE', #13832, #10679 ) ;
#15440 = CARTESIAN_POINT ( 'NONE',  ( 5.571366797620176392, 51.37294568574342435, 77.09285305542944400 ) ) ;
#15441 = CARTESIAN_POINT ( 'NONE',  ( 9.131267103411046193, 42.16071128789349132, 78.09998440036279987 ) ) ;
#15442 = CARTESIAN_POINT ( 'NONE',  ( 1.256812508749381774, 49.74246873332880625, 92.67996380294498238 ) ) ;
#15443 = CARTESIAN_POINT ( 'NONE',  ( 1.514255888186003984, 52.36218137147968577, 87.21440135111343750 ) ) ;
#15444 = CARTESIAN_POINT ( 'NONE',  ( -3.652148518534829247, 36.30515569394113129, 77.93013364623398331 ) ) ;
#15445 = CARTESIAN_POINT ( 'NONE',  ( 4.134898411747151670, 47.90306806511021875, 95.05422504033560926 ) ) ;
#15446 = DIRECTION ( 'NONE',  ( 1.540237394707284220E-16, 1.793354297423764243E-16, -1.000000000000000000 ) ) ;
#15447 = DIRECTION ( 'NONE',  ( -3.893792155548169402E-16, -7.183611964723547524E-17, 1.000000000000000000 ) ) ;
#15448 = ORIENTED_EDGE ( 'NONE', *, *, #1941, .F. ) ;
#15449 = CARTESIAN_POINT ( 'NONE',  ( 5.939849532777430774, 51.10076233267274404, 76.96076274685535168 ) ) ;
#15450 = ORIENTED_EDGE ( 'NONE', *, *, #8083, .F. ) ;
#15451 = EDGE_CURVE ( 'NONE', #14291, #16499, #440, .T. ) ;
#15452 = CARTESIAN_POINT ( 'NONE',  ( -4.424094442032265206, 50.69663029939598431, 78.82882669246485818 ) ) ;
#15453 = CARTESIAN_POINT ( 'NONE',  ( 4.454347278305088587, 39.79502279609036464, 90.11785590924256439 ) ) ;
#15454 = VERTEX_POINT ( 'NONE', #12573 ) ;
#15455 = CARTESIAN_POINT ( 'NONE',  ( 2.122153740306507608, 49.76218137147969856, 85.55433879953100984 ) ) ;
#15456 = LINE ( 'NONE', #13534, #17961 ) ;
#15457 = CARTESIAN_POINT ( 'NONE',  ( -3.373742936343101739, 52.19408846175863204, 78.58955347608575437 ) ) ;
#15458 = CARTESIAN_POINT ( 'NONE',  ( 0.8019072594418875655, 52.95773867775533716, 77.48431196819693412 ) ) ;
#15459 = CARTESIAN_POINT ( 'NONE',  ( 0.3395551853511908913, 52.36014964445268305, 77.58553591360387713 ) ) ;
#15460 = DIRECTION ( 'NONE',  ( -0.5941461771851693774, -0.8043570849667760481, -2.357623395011396791E-16 ) ) ;
#15461 = VERTEX_POINT ( 'NONE', #9493 ) ;
#15462 = CARTESIAN_POINT ( 'NONE',  ( 5.262940487106410714, 50.85284745661634531, 78.03948491463276582 ) ) ;
#15463 = EDGE_CURVE ( 'NONE', #3020, #2188, #8224, .T. ) ;
#15464 = EDGE_LOOP ( 'NONE', ( #7523, #17806, #11716, #5324 ) ) ;
#15465 = CARTESIAN_POINT ( 'NONE',  ( -1.174478664588461951, 57.66640723084523046, 54.55433879953099563 ) ) ;
#15466 = CARTESIAN_POINT ( 'NONE',  ( 4.539621438837683876, 52.13505442103787857, 76.64209438045911327 ) ) ;
#15467 = CARTESIAN_POINT ( 'NONE',  ( 2.119851040271389930, 52.81592988514039178, 78.16610350541323271 ) ) ;
#15468 = CARTESIAN_POINT ( 'NONE',  ( 0.5221537403065017457, 49.16218137147969003, 92.45433879953097289 ) ) ;
#15469 = CARTESIAN_POINT ( 'NONE',  ( 7.862039597456297102, 47.81814697137103565, 79.15362846919002493 ) ) ;
#15470 = ADVANCED_FACE ( 'NONE', ( #19065 ), #367, .T. ) ;
#15471 = LINE ( 'NONE', #17269, #11185 ) ;
#15472 = CARTESIAN_POINT ( 'NONE',  ( 0.2541436421823696223, 38.02374091943176637, 95.45433879782399345 ) ) ;
#15473 = DIRECTION ( 'NONE',  ( -0.9534635866061452747, -0.3015081906286225522, -2.009271279954815797E-16 ) ) ;
#15474 = B_SPLINE_SURFACE_WITH_KNOTS ( 'NONE', 3, 1, ( 
 ( #5003, #4584 ),
 ( #9507, #15991 ),
 ( #8106, #14596 ),
 ( #16303, #1735 ),
 ( #14699, #13108 ),
 ( #19894, #12048 ),
 ( #3420, #3837 ),
 ( #7018, #18418 ),
 ( #9931, #3527 ),
 ( #15020, #8648 ),
 ( #19993, #18205 ),
 ( #10031, #5315 ),
 ( #2038, #3625 ),
 ( #13214, #8535 ),
 ( #6708, #10358 ),
 ( #11831, #16828 ),
 ( #16414, #10135 ),
 ( #13519, #439 ),
 ( #6922, #16724 ),
 ( #222, #16617 ),
 ( #1837, #645 ),
 ( #13323, #5216 ),
 ( #14798, #13426 ) ),
 .UNSPECIFIED., .F., .F., .F.,
 ( 4, 1, 1, 1, 1, 1, 1, 1, 1, 1, 1, 1, 1, 1, 1, 1, 1, 1, 1, 1, 4 ),
 ( 2, 2 ),
 ( 0.000000000000000000, 0.04996570031508023452, 0.09882111805538688898, 0.1466986691414003396, 0.1933343388926866968, 0.2389025989959846497, 0.2841336389028531473, 0.3290918654023432532, 0.3737715338516285901, 0.4170420466396844161, 0.4581370997277735002, 0.4966756662638874276, 0.5332138716254802846, 0.5686376898124313461, 0.6026332556748308367, 0.6353084426624004966, 0.6676556782331927176, 0.7363269649188709520, 0.8138826302435128168, 0.9017756963292008487, 1.000000000000000000 ),
 ( 0.000000000000000000, 1.000000000000000000 ),
 .UNSPECIFIED. ) ;
#15475 = ORIENTED_EDGE ( 'NONE', *, *, #2496, .F. ) ;
#15476 = CARTESIAN_POINT ( 'NONE',  ( -7.677846259693480668, 36.96218137147968008, 93.55433879953098142 ) ) ;
#15477 = EDGE_CURVE ( 'NONE', #13124, #14061, #4475, .T. ) ;
#15478 = EDGE_CURVE ( 'NONE', #7860, #10020, #19161, .T. ) ;
#15479 = ORIENTED_EDGE ( 'NONE', *, *, #6250, .F. ) ;
#15480 = DIRECTION ( 'NONE',  ( -1.000000000000000000, -1.402518428993809490E-16, 6.308085367188358884E-15 ) ) ;
#15481 = ADVANCED_FACE ( 'NONE', ( #19653 ), #11594, .F. ) ;
#15482 = CARTESIAN_POINT ( 'NONE',  ( 3.122153740306552905, 48.66551347115873227, 94.78933879953099506 ) ) ;
#15483 = CARTESIAN_POINT ( 'NONE',  ( -8.139710801171299082, 42.34786680499500733, 76.77997794206987692 ) ) ;
#15484 = ORIENTED_EDGE ( 'NONE', *, *, #19875, .F. ) ;
#15485 = CARTESIAN_POINT ( 'NONE',  ( -5.154188915835984375, 42.64120994080404614, 93.61746380123797451 ) ) ;
#15486 = CARTESIAN_POINT ( 'NONE',  ( -4.622577041588897373, 46.56120873422322859, 94.90746379782396502 ) ) ;
#15487 = LINE ( 'NONE', #16866, #2486 ) ;
#15488 = ORIENTED_EDGE ( 'NONE', *, *, #3595, .T. ) ;
#15489 = CARTESIAN_POINT ( 'NONE',  ( 5.201216021426783520, 36.68989574863261538, 75.41205140984322952 ) ) ;
#15490 = CARTESIAN_POINT ( 'NONE',  ( -0.9504375969237850441, 51.37401713635502887, 77.21536821129558348 ) ) ;
#15491 = ADVANCED_FACE ( 'NONE', ( #11490 ), #1804, .F. ) ;
#15492 = VERTEX_POINT ( 'NONE', #18071 ) ;
#15493 = CARTESIAN_POINT ( 'NONE',  ( 1.132007891697332846, 52.34004019480227754, 79.51057667246605831 ) ) ;
#15494 = CARTESIAN_POINT ( 'NONE',  ( 6.828503391016846891, 43.33193468930419101, 90.41433880123798872 ) ) ;
#15495 = ORIENTED_EDGE ( 'NONE', *, *, #10415, .T. ) ;
#15496 = CARTESIAN_POINT ( 'NONE',  ( -4.342627717588348091, 41.70135421888197413, 92.45433879953091605 ) ) ;
#15497 = LINE ( 'NONE', #908, #6103 ) ;
#15498 = FACE_OUTER_BOUND ( 'NONE', #3645, .T. ) ;
#15499 = ITEM_DEFINED_TRANSFORMATION ( 'NONE', 'NONE', #16674,  #18366 ) ;
#15500 = CARTESIAN_POINT ( 'NONE',  ( -3.533008836142935927, 36.21715200979740246, 78.43912781517941823 ) ) ;
#15501 = CARTESIAN_POINT ( 'NONE',  ( 5.317959575120520199, 50.80701191653712101, 78.92241520643889885 ) ) ;
#15502 = DIRECTION ( 'NONE',  ( -1.402518428993831430E-16, 1.000000000000000000, -2.891205793294680792E-16 ) ) ;
#15503 = ORIENTED_EDGE ( 'NONE', *, *, #4183, .F. ) ;
#15504 = CARTESIAN_POINT ( 'NONE',  ( 2.100548972721439256, 52.95446970717261337, 76.22990676838142576 ) ) ;
#15505 = VERTEX_POINT ( 'NONE', #1898 ) ;
#15506 = CARTESIAN_POINT ( 'NONE',  ( -0.8350644498690075190, 52.24919065719213762, 78.94532217087298420 ) ) ;
#15507 = EDGE_CURVE ( 'NONE', #15510, #1549, #3489, .T. ) ;
#15508 = DIRECTION ( 'NONE',  ( -1.571217453038212812E-16, -0.7071067811865525687, -0.7071067811865425767 ) ) ;
#15509 = CARTESIAN_POINT ( 'NONE',  ( -5.784195910403845176, 44.99242805365518194, 94.63308880123798872 ) ) ;
#15510 = VERTEX_POINT ( 'NONE', #16477 ) ;
#15511 = ADVANCED_FACE ( 'NONE', ( #10097 ), #8498, .F. ) ;
#15512 = CARTESIAN_POINT ( 'NONE',  ( 6.117874454611452961, 50.05524748896710463, 79.34836068132329956 ) ) ;
#15513 = EDGE_LOOP ( 'NONE', ( #10522, #8553, #9026, #17101 ) ) ;
#15514 = CARTESIAN_POINT ( 'NONE',  ( 4.335841838902815937, 51.37156319753863443, 79.19424447893550223 ) ) ;
#15515 = CARTESIAN_POINT ( 'NONE',  ( 0.5221537403065014127, 44.16218137147968292, 76.16022115247204738 ) ) ;
#15516 = CARTESIAN_POINT ( 'NONE',  ( -3.467962453771610054, 40.50591351489412517, 91.00121379953098710 ) ) ;
#15517 = CARTESIAN_POINT ( 'NONE',  ( -4.517974409599069041, 36.94470640207596546, 78.25995115514949418 ) ) ;
#15518 = CARTESIAN_POINT ( 'NONE',  ( -4.383473025373058718, 51.47257230871590394, 76.47051527011910821 ) ) ;
#15519 = CARTESIAN_POINT ( 'NONE',  ( -0.1944850259765472933, 35.99355670886600933, 76.86610350541323555 ) ) ;
#15520 = CARTESIAN_POINT ( 'NONE',  ( -5.784195910403845176, 44.99242805365518194, 96.03933880123796030 ) ) ;
#15521 = DIRECTION ( 'NONE',  ( 0.9429220365244121993, -0.3330135628418984250, 8.551124769255302663E-17 ) ) ;
#15522 = CARTESIAN_POINT ( 'NONE',  ( -5.403172002243911365, 49.82415717112796472, 76.65235776097600251 ) ) ;
#15523 = CARTESIAN_POINT ( 'NONE',  ( 4.942331607238935831, 51.83758864179496584, 75.54250430092201896 ) ) ;
#15524 = EDGE_CURVE ( 'NONE', #14895, #18369, #5502, .T. ) ;
#15525 = CARTESIAN_POINT ( 'NONE',  ( -4.500660556396669065, 42.81632233694663370, 93.07058880294496817 ) ) ;
#15526 = CARTESIAN_POINT ( 'NONE',  ( -7.302004416484622951, 40.13443851219999914, 78.72624606083481069 ) ) ;
#15527 = CARTESIAN_POINT ( 'NONE',  ( 8.951433321995803993, 41.62173803654965099, 78.54183882225588320 ) ) ;
#15528 = AXIS2_PLACEMENT_3D ( 'NONE', #12113, #2316, #15306 ) ;
#15529 = VERTEX_POINT ( 'NONE', #7084 ) ;
#15530 = FACE_OUTER_BOUND ( 'NONE', #4438, .T. ) ;
#15531 = CARTESIAN_POINT ( 'NONE',  ( 5.722153740306818115, 44.84677435893292596, 93.35825776475003579 ) ) ;
#15532 = CARTESIAN_POINT ( 'NONE',  ( -4.539611090124166637, 51.36100176422416297, 79.54777180229389444 ) ) ;
#15533 = CARTESIAN_POINT ( 'NONE',  ( 3.460444912181559474, 49.25145096859824889, 90.64871380123798872 ) ) ;
#15534 = CARTESIAN_POINT ( 'NONE',  ( -4.570740025688047048, 36.98368223715222314, 77.15538146413656762 ) ) ;
#15535 = CARTESIAN_POINT ( 'NONE',  ( -7.604387687253306716, 43.11263983757604024, 78.56936110682462981 ) ) ;
#15536 = CARTESIAN_POINT ( 'NONE',  ( 8.647930352917317265, 43.06138273419885820, 77.20731746004976515 ) ) ;
#15537 = CARTESIAN_POINT ( 'NONE',  ( -4.219041845479045705, 37.47853290070158039, 76.02016401025396419 ) ) ;
#15538 = ORIENTED_EDGE ( 'NONE', *, *, #4025, .T. ) ;
#15539 = VERTEX_POINT ( 'NONE', #18487 ) ;
#15540 = CARTESIAN_POINT ( 'NONE',  ( 8.279961632505596469, 41.50566914870238122, 78.93448121625959857 ) ) ;
#15541 = CARTESIAN_POINT ( 'NONE',  ( 8.787829143201870252, 41.13140593384865440, 77.14698585835439815 ) ) ;
#15542 = CARTESIAN_POINT ( 'NONE',  ( 8.921551879414991504, 41.53218145749156776, 76.03029119948048731 ) ) ;
#15543 = FACE_OUTER_BOUND ( 'NONE', #10049, .T. ) ;
#15544 = CARTESIAN_POINT ( 'NONE',  ( 5.349754812510225221, 50.78352605546763954, 77.95044976498417100 ) ) ;
#15545 = B_SPLINE_CURVE_WITH_KNOTS ( 'NONE', 3,
 ( #20012, #2485, #777, #7259, #15462, #15568, #8764, #11850 ),
 .UNSPECIFIED., .F., .F.,
 ( 4, 2, 2, 4 ),
 ( 0.000000000000000000, 0.0001162705178784993038, 0.0002325410357569986076, 0.0004650820715139567202 ),
 .UNSPECIFIED. ) ;
#15546 = VECTOR ( 'NONE', #13620, 1000.000000000000000 ) ;
#15547 = CARTESIAN_POINT ( 'NONE',  ( 8.421385860420697256, 42.39757021913804635, 78.09998440036279987 ) ) ;
#15548 = CARTESIAN_POINT ( 'NONE',  ( 3.948530577815480225, 39.69684013992245752, 90.96121380294498238 ) ) ;
#15549 = DIRECTION ( 'NONE',  ( -1.779391786395883783E-16, -5.922860397471806844E-17, 1.000000000000000000 ) ) ;
#15550 = CARTESIAN_POINT ( 'NONE',  ( 30.92220646078100188, 45.56218137147968861, 56.80715055817104542 ) ) ;
#15551 = CARTESIAN_POINT ( 'NONE',  ( 5.611423337425062385, 41.22389019960463230, 91.42996380123798872 ) ) ;
#15552 = VECTOR ( 'NONE', #2560, 1000.000000000000000 ) ;
#15553 = CARTESIAN_POINT ( 'NONE',  ( 2.522153740306505298, 49.16218137147968292, 82.55433879953099563 ) ) ;
#15554 = EDGE_LOOP ( 'NONE', ( #1936, #19674, #448, #15117 ) ) ;
#15555 = CARTESIAN_POINT ( 'NONE',  ( 5.547944990773469698, 50.63561048897027916, 77.19464465032660883 ) ) ;
#15556 = EDGE_LOOP ( 'NONE', ( #19805, #16517, #16932, #9838 ) ) ;
#15557 = VECTOR ( 'NONE', #17840, 1000.000000000000000 ) ;
#15558 = CARTESIAN_POINT ( 'NONE',  ( -4.802657821332910082, 51.17303820085790278, 78.59458524649963351 ) ) ;
#15559 = CARTESIAN_POINT ( 'NONE',  ( 6.102441102155617969, 43.42752260303680600, 92.36746380294498238 ) ) ;
#15560 = ORIENTED_EDGE ( 'NONE', *, *, #13589, .T. ) ;
#15561 = CARTESIAN_POINT ( 'NONE',  ( 2.522153740306506631, 49.16218137147969003, 74.55433879953100984 ) ) ;
#15562 = DIRECTION ( 'NONE',  ( 1.193617070626243484E-16, 1.000000000000000000, 0.000000000000000000 ) ) ;
#15563 = CARTESIAN_POINT ( 'NONE',  ( 0.3821786226492924210, 35.36301154328572949, 78.57639762306027365 ) ) ;
#15564 = CARTESIAN_POINT ( 'NONE',  ( -1.493738069816089364, 38.45421922485636657, 75.45433879953087342 ) ) ;
#15565 = CARTESIAN_POINT ( 'NONE',  ( 2.522153740306505298, 50.16218137147969713, 85.15433879953098995 ) ) ;
#15566 = DIRECTION ( 'NONE',  ( 1.000000000000000000, 0.000000000000000000, 0.000000000000000000 ) ) ;
#15567 = VERTEX_POINT ( 'NONE', #13586 ) ;
#15568 = CARTESIAN_POINT ( 'NONE',  ( 5.242206828355853609, 50.86750652479793189, 78.15346193224233673 ) ) ;
#15569 = AXIS2_PLACEMENT_3D ( 'NONE', #19151, #9378, #15861 ) ;
#15570 = VERTEX_POINT ( 'NONE', #6978 ) ;
#15571 = DIRECTION ( 'NONE',  ( -0.9534635866061452747, -0.3015081906286226077, -2.009271279954815304E-16 ) ) ;
#15572 = DIRECTION ( 'NONE',  ( 0.000000000000000000, 0.000000000000000000, -1.000000000000000000 ) ) ;
#15573 = ADVANCED_FACE ( 'NONE', ( #10525 ), #7310, .T. ) ;
#15574 = LINE ( 'NONE', #8769, #15643 ) ;
#15575 = CARTESIAN_POINT ( 'NONE',  ( -7.292692585215720946, 46.64628091931714948, 79.36031032450011935 ) ) ;
#15576 = CARTESIAN_POINT ( 'NONE',  ( 8.787829143201870252, 41.13140593384865440, 78.45948585835439815 ) ) ;
#15577 = CARTESIAN_POINT ( 'NONE',  ( -4.322630238256937041, 37.54627981234005318, 77.92970022298523247 ) ) ;
#15578 = CARTESIAN_POINT ( 'NONE',  ( 5.277046726144507538, 37.48121749977929795, 78.28595324781899478 ) ) ;
#15579 = VERTEX_POINT ( 'NONE', #18696 ) ;
#15580 = FACE_OUTER_BOUND ( 'NONE', #10296, .T. ) ;
#15581 = CIRCLE ( 'NONE', #3675, 8.199999999999995737 ) ;
#15582 = ORIENTED_EDGE ( 'NONE', *, *, #8155, .F. ) ;
#15583 = DIRECTION ( 'NONE',  ( 0.000000000000000000, 0.000000000000000000, 1.000000000000000000 ) ) ;
#15584 = ADVANCED_FACE ( 'NONE', ( #9025 ), #501, .T. ) ;
#15585 = CARTESIAN_POINT ( 'NONE',  ( -5.154188915835984375, 42.64120994080404614, 94.86746380123797451 ) ) ;
#15586 = CARTESIAN_POINT ( 'NONE',  ( -7.398469273655679856, 42.45442617122637330, 76.93555611204594413 ) ) ;
#15587 = EDGE_LOOP ( 'NONE', ( #7568, #20436, #7459, #16964 ) ) ;
#15588 = CARTESIAN_POINT ( 'NONE',  ( -4.524181921268124462, 40.28999182795290324, 94.94558880123797451 ) ) ;
#15589 = CARTESIAN_POINT ( 'NONE',  ( 2.447781712115293828, 38.42313889284341144, 75.45433879953087342 ) ) ;
#15590 = FACE_BOUND ( 'NONE', #11563, .T. ) ;
#15591 = ORIENTED_EDGE ( 'NONE', *, *, #18320, .T. ) ;
#15592 = DIRECTION ( 'NONE',  ( 0.2896293787568423594, -0.9158990529585747664, 0.2779275944387522568 ) ) ;
#15593 = CARTESIAN_POINT ( 'NONE',  ( 0.5221537403065181771, 44.16218137147969003, 56.15433879953099705 ) ) ;
#15594 = EDGE_CURVE ( 'NONE', #4812, #10826, #604, .T. ) ;
#15595 = ORIENTED_EDGE ( 'NONE', *, *, #18075, .F. ) ;
#15596 = DIRECTION ( 'NONE',  ( -1.540237394707284467E-16, -1.793354297423764243E-16, 1.000000000000000000 ) ) ;
#15597 = CARTESIAN_POINT ( 'NONE',  ( 0.7971270633857517884, 52.35255750736508418, 78.82560697059345500 ) ) ;
#15598 = ORIENTED_EDGE ( 'NONE', *, *, #13251, .F. ) ;
#15599 = CARTESIAN_POINT ( 'NONE',  ( -5.329330622855473543, 49.90705297800482754, 78.91939974476616726 ) ) ;
#15600 = CARTESIAN_POINT ( 'NONE',  ( 5.122276503711423956, 37.37399599821077345, 76.07344584094424533 ) ) ;
#15601 = EDGE_CURVE ( 'NONE', #8055, #476, #18378, .T. ) ;
#15602 = CARTESIAN_POINT ( 'NONE',  ( 2.043125170982144745, 38.48583871533720213, 91.27371380123798872 ) ) ;
#15603 = VECTOR ( 'NONE', #2464, 1000.000000000000000 ) ;
#15604 = ITEM_DEFINED_TRANSFORMATION ( 'NONE', 'NONE', #12932,  #18366 ) ;
#15605 = CARTESIAN_POINT ( 'NONE',  ( 5.438900134727234992, 36.85973611382630821, 76.29939265556315320 ) ) ;
#15606 = CARTESIAN_POINT ( 'NONE',  ( 5.521494261397323022, 36.91875485278077207, 76.01263398532663018 ) ) ;
#15607 = DIRECTION ( 'NONE',  ( -0.3165065846431826535, -0.9485903129789527988, 0.000000000000000000 ) ) ;
#15608 = ORIENTED_EDGE ( 'NONE', *, *, #13786, .T. ) ;
#15609 = EDGE_CURVE ( 'NONE', #14794, #6491, #2310, .T. ) ;
#15610 = CARTESIAN_POINT ( 'NONE',  ( 1.472692277483312218, 52.20658247672307795, 75.49332451037695080 ) ) ;
#15611 = EDGE_LOOP ( 'NONE', ( #1949, #19578, #20864, #6713, #16823, #5520, #13531, #9953 ) ) ;
#15612 = CARTESIAN_POINT ( 'NONE',  ( 30.92220646078100188, 45.56218137147968861, 62.80715055817104542 ) ) ;
#15613 = DIRECTION ( 'NONE',  ( 1.000000000000000000, 0.000000000000000000, 0.000000000000000000 ) ) ;
#15614 = CARTESIAN_POINT ( 'NONE',  ( 6.828503391016846891, 43.33193468930419101, 90.41433880123798872 ) ) ;
#15615 = ORIENTED_EDGE ( 'NONE', *, *, #18306, .F. ) ;
#15616 = AXIS2_PLACEMENT_3D ( 'NONE', #6933, #13437, #17804 ) ;
#15617 = VERTEX_POINT ( 'NONE', #2530 ) ;
#15618 = FACE_OUTER_BOUND ( 'NONE', #13333, .T. ) ;
#15619 = ORIENTED_EDGE ( 'NONE', *, *, #14847, .F. ) ;
#15620 = DIRECTION ( 'NONE',  ( 1.779391786395883536E-16, 5.922860397471805611E-17, -1.000000000000000000 ) ) ;
#15621 = DIRECTION ( 'NONE',  ( -0.5941461771851692664, -0.8043570849667761591, -2.357623395011396791E-16 ) ) ;
#15622 = CARTESIAN_POINT ( 'NONE',  ( 8.385851074499695912, 39.92665216093506331, 76.98031643592585738 ) ) ;
#15623 = VECTOR ( 'NONE', #13801, 1000.000000000000000 ) ;
#15624 = ORIENTED_EDGE ( 'NONE', *, *, #14790, .F. ) ;
#15625 = DIRECTION ( 'NONE',  ( 0.9999689119394085113, -0.007885122365285377952, 1.526048693634335642E-16 ) ) ;
#15626 = CARTESIAN_POINT ( 'NONE',  ( -7.511311626346421022, 40.36128364442370042, 79.17963929739188700 ) ) ;
#15627 = LINE ( 'NONE', #2537, #5085 ) ;
#15628 = CARTESIAN_POINT ( 'NONE',  ( 5.611423337425062385, 41.22389019960463230, 91.58621380123798872 ) ) ;
#15629 = CARTESIAN_POINT ( 'NONE',  ( 0.5221537403065015237, 44.16218137147968292, 75.45433879953087342 ) ) ;
#15630 = EDGE_CURVE ( 'NONE', #18174, #15290, #12109, .T. ) ;
#15631 = VECTOR ( 'NONE', #9003, 1000.000000000000114 ) ;
#15632 = CARTESIAN_POINT ( 'NONE',  ( -5.569494948991628114, 50.62508446513216143, 75.69846806870741318 ) ) ;
#15633 = CARTESIAN_POINT ( 'NONE',  ( -2.077846259693550746, 39.65884927180063357, 94.47683880294496817 ) ) ;
#15634 = EDGE_CURVE ( 'NONE', #1549, #597, #8808, .T. ) ;
#15635 = CARTESIAN_POINT ( 'NONE',  ( -0.2125050281363792815, 38.58189400963055959, 90.80496380294498238 ) ) ;
#15636 = VECTOR ( 'NONE', #6252, 1000.000000000000000 ) ;
#15637 = CARTESIAN_POINT ( 'NONE',  ( -7.777085147165724521, 41.23087250612003629, 79.53766176265342835 ) ) ;
#15638 = ADVANCED_FACE ( 'NONE', ( #12212 ), #11603, .T. ) ;
#15639 = CARTESIAN_POINT ( 'NONE',  ( 8.950289981099260217, 41.61831137135051506, 78.71610475470291135 ) ) ;
#15640 = EDGE_CURVE ( 'NONE', #6443, #10025, #9558, .T. ) ;
#15641 = CIRCLE ( 'NONE', #14263, 8.199999999999995737 ) ;
#15642 = DIRECTION ( 'NONE',  ( 1.540237394707283727E-16, 1.793354297423763257E-16, -1.000000000000000000 ) ) ;
#15643 = VECTOR ( 'NONE', #13759, 1000.000000000000000 ) ;
#15644 = DIRECTION ( 'NONE',  ( 1.540237394707284220E-16, 1.793354297423764243E-16, -1.000000000000000000 ) ) ;
#15645 = CARTESIAN_POINT ( 'NONE',  ( -3.926839636664805511, 51.79886580987140832, 79.42193487995672285 ) ) ;
#15646 =( LENGTH_UNIT ( ) NAMED_UNIT ( * ) SI_UNIT ( .MILLI., .METRE. ) );
#15647 = CARTESIAN_POINT ( 'NONE',  ( -8.309364629785569889, 42.88970911912626605, 78.56936110682462981 ) ) ;
#15648 = CARTESIAN_POINT ( 'NONE',  ( 0.5221537403065015237, 44.16218137147968292, 75.45433879953088763 ) ) ;
#15649 = AXIS2_PLACEMENT_3D ( 'NONE', #20255, #8690, #702 ) ;
#15650 = ORIENTED_EDGE ( 'NONE', *, *, #14055, .F. ) ;
#15651 = VECTOR ( 'NONE', #13143, 1000.000000000000227 ) ;
#15652 = CARTESIAN_POINT ( 'NONE',  ( 9.347650859976274873, 42.80922713344904196, 78.67881838835081965 ) ) ;
#15653 = CARTESIAN_POINT ( 'NONE',  ( -4.152600114974411838, 50.89932002992104998, 75.97646144330421691 ) ) ;
#15654 = CARTESIAN_POINT ( 'NONE',  ( 1.514255888186008425, 52.36218137147968577, 52.53721119516358584 ) ) ;
#15655 = CARTESIAN_POINT ( 'NONE',  ( 5.908589799165438805, 51.12385263867304275, 77.19464465032660883 ) ) ;
#15656 = B_SPLINE_SURFACE_WITH_KNOTS ( 'NONE', 3, 1, ( 
 ( #9067, #10685 ),
 ( #7674, #866 ),
 ( #2568, #12053 ),
 ( #3945, #18845 ),
 ( #9287, #4358 ),
 ( #13841, #15666 ),
 ( #17045, #15555 ),
 ( #7350, #7574 ),
 ( #8964, #20111 ),
 ( #971, #10469 ),
 ( #16933, #15347 ),
 ( #10884, #7246 ),
 ( #15449, #20437 ),
 ( #12370, #4256 ),
 ( #5645, #2784 ) ),
 .UNSPECIFIED., .F., .F., .F.,
 ( 4, 1, 1, 1, 1, 1, 1, 1, 1, 1, 1, 1, 4 ),
 ( 2, 2 ),
 ( 0.000000000000000000, 0.1112587825215290704, 0.2075697215801151074, 0.2973595701983123840, 0.3838682041569268510, 0.4304545292676484891, 0.4853887544929457731, 0.5479167518276804039, 0.6204346596782769341, 0.7008860551074163059, 0.7907659637769564043, 0.8904818903857688595, 1.000000000000000000 ),
 ( 0.000000000000000000, 1.000000000000000000 ),
 .UNSPECIFIED. ) ;
#15657 = DIRECTION ( 'NONE',  ( -1.334402673828316297E-16, 2.168404344970984808E-15, 1.000000000000000000 ) ) ;
#15658 = VECTOR ( 'NONE', #1289, 1000.000000000000000 ) ;
#15659 = CARTESIAN_POINT ( 'NONE',  ( 8.532965227243460404, 42.73198065996890449, 77.95057265855270145 ) ) ;
#15660 = CARTESIAN_POINT ( 'NONE',  ( -0.07555581626192474365, 50.25084051303456789, 53.06567965797612629 ) ) ;
#15661 = EDGE_CURVE ( 'NONE', #1211, #11865, #19145, .T. ) ;
#15662 = CARTESIAN_POINT ( 'NONE',  ( 2.043125170982144745, 38.48583871533720213, 92.52371380123798872 ) ) ;
#15663 = AXIS2_PLACEMENT_3D ( 'NONE', #9987, #17949, #10300 ) ;
#15664 = CARTESIAN_POINT ( 'NONE',  ( -4.359893715479207899, 37.57388776543446340, 75.36022115247205022 ) ) ;
#15665 = ORIENTED_EDGE ( 'NONE', *, *, #8352, .T. ) ;
#15666 = CARTESIAN_POINT ( 'NONE',  ( 5.534096227355138176, 50.64584001264518065, 77.22227766523002401 ) ) ;
#15667 = VERTEX_POINT ( 'NONE', #7412 ) ;
#15668 = STYLED_ITEM ( 'NONE', ( #8824 ), #4882 ) ;
#15669 = LINE ( 'NONE', #12775, #6120 ) ;
#15670 = CARTESIAN_POINT ( 'NONE',  ( -0.8237052942265477018, 49.18499566818285018, 94.00808880294498238 ) ) ;
#15671 = ORIENTED_EDGE ( 'NONE', *, *, #10579, .T. ) ;
#15672 = CARTESIAN_POINT ( 'NONE',  ( 2.463659247115866258, 38.82793883177424732, 94.28246379782397923 ) ) ;
#15673 = CARTESIAN_POINT ( 'NONE',  ( -0.8988261294859191119, 52.21915217126601050, 76.13122899883298089 ) ) ;
#15674 = CARTESIAN_POINT ( 'NONE',  ( 8.850612593395874583, 41.31957191698789700, 78.01079203130994699 ) ) ;
#15675 = CARTESIAN_POINT ( 'NONE',  ( 0.5221537403065006355, 44.16218137147969003, 92.45433879953097289 ) ) ;
#15676 = PLANE ( 'NONE',  #7718 ) ;
#15677 = CARTESIAN_POINT ( 'NONE',  ( -4.895593109503408868, 37.22363812428621088, 78.53742703482498655 ) ) ;
#15678 = ORIENTED_EDGE ( 'NONE', *, *, #7288, .F. ) ;
#15679 = PLANE ( 'NONE',  #10207 ) ;
#15680 = ORIENTED_EDGE ( 'NONE', *, *, #647, .T. ) ;
#15681 = DIRECTION ( 'NONE',  ( 0.000000000000000000, -1.000000000000000000, 0.000000000000000000 ) ) ;
#15682 = CARTESIAN_POINT ( 'NONE',  ( 31.07218010054375412, 42.76218137147968434, 66.20574467885103331 ) ) ;
#15683 = CARTESIAN_POINT ( 'NONE',  ( -2.416137431568557314, 39.07291177436112406, 93.61746380123797451 ) ) ;
#15684 = LINE ( 'NONE', #1307, #9646 ) ;
#15685 = PLANE ( 'NONE',  #12870 ) ;
#15686 = CARTESIAN_POINT ( 'NONE',  ( -4.158578283022523969, 37.42937009194850617, 78.34992703482498655 ) ) ;
#15687 = CARTESIAN_POINT ( 'NONE',  ( -4.756616962678585026, 37.12098204292738757, 75.36046818803191627 ) ) ;
#15688 = AXIS2_PLACEMENT_3D ( 'NONE', #10991, #17462, #6481 ) ;
#15689 = B_SPLINE_CURVE_WITH_KNOTS ( 'NONE', 3,
 ( #14032, #20405, #9039, #15844, #15526, #5836, #12342, #12540, #17330, #2648, #1368, #941, #18820, #15637, #20513, #7857 ),
 .UNSPECIFIED., .F., .F.,
 ( 4, 2, 2, 2, 2, 2, 2, 4 ),
 ( 0.000000000000000000, 0.0001315995296408621585, 0.0002631990592817243170, 0.0005263981185634489593, 0.0007895971778451736558, 0.001052796237126898135, 0.001579194355690331482, 0.002105592474253764612 ),
 .UNSPECIFIED. ) ;
#15690 = VERTEX_POINT ( 'NONE', #17312 ) ;
#15691 = CARTESIAN_POINT ( 'NONE',  ( 0.5221537403065008576, 44.16218137147968292, 80.45433879953087342 ) ) ;
#15692 = AXIS2_PLACEMENT_3D ( 'NONE', #224, #330, #4900 ) ;
#15693 = EDGE_LOOP ( 'NONE', ( #19008, #19116, #3760, #18759 ) ) ;
#15694 = LINE ( 'NONE', #17276, #7481 ) ;
#15695 = CARTESIAN_POINT ( 'NONE',  ( 5.568489401881125289, 48.03437091500646261, 94.32058880123798872 ) ) ;
#15696 = CARTESIAN_POINT ( 'NONE',  ( 5.531249400824703955, 51.40257879072892422, 75.36789977960694387 ) ) ;
#15697 = ORIENTED_EDGE ( 'NONE', *, *, #18545, .F. ) ;
#15698 = EDGE_CURVE ( 'NONE', #9664, #4990, #10279, .T. ) ;
#15699 = CARTESIAN_POINT ( 'NONE',  ( 5.568489401881125289, 48.03437091500646261, 94.32058880123798872 ) ) ;
#15700 = LINE ( 'NONE', #16109, #3150 ) ;
#15701 = CARTESIAN_POINT ( 'NONE',  ( -4.517072128342573656, 36.94403992325788977, 78.58080938776616620 ) ) ;
#15702 = LINE ( 'NONE', #18984, #17973 ) ;
#15703 = ORIENTED_EDGE ( 'NONE', *, *, #11293, .T. ) ;
#15704 = CARTESIAN_POINT ( 'NONE',  ( 5.025485839985549319, 41.56218137147963887, 93.22683879953099506 ) ) ;
#15705 = CARTESIAN_POINT ( 'NONE',  ( -5.917125461193805336, 40.64525615903904310, 75.45433879953087342 ) ) ;
#15706 = VECTOR ( 'NONE', #14943, 1000.000000000000000 ) ;
#15707 = ORIENTED_EDGE ( 'NONE', *, *, #634, .F. ) ;
#15708 = CARTESIAN_POINT ( 'NONE',  ( -0.7071044773352802570, 39.15572691966126229, 92.45433879953097289 ) ) ;
#15709 = DIRECTION ( 'NONE',  ( -1.402518428993830937E-16, 1.000000000000000000, -3.469446951953617147E-16 ) ) ;
#15710 =( GEOMETRIC_REPRESENTATION_CONTEXT ( 3 ) GLOBAL_UNCERTAINTY_ASSIGNED_CONTEXT ( ( #9772 ) ) GLOBAL_UNIT_ASSIGNED_CONTEXT ( ( #15646, #12547, #7438 ) ) REPRESENTATION_CONTEXT ( 'NONE', 'WORKASPACE' ) );
#15711 = CARTESIAN_POINT ( 'NONE',  ( -3.628867371436365730, 48.69222599884265179, 94.98558879782399345 ) ) ;
#15712 = ADVANCED_FACE ( 'NONE', ( #20389 ), #18906, .F. ) ;
#15713 = ITEM_DEFINED_TRANSFORMATION ( 'NONE', 'NONE', #6463,  #18366 ) ;
#15714 = CARTESIAN_POINT ( 'NONE',  ( 5.434476177758928550, 36.85657491614816195, 76.36627918048426977 ) ) ;
#15715 = CARTESIAN_POINT ( 'NONE',  ( 8.790110392356673685, 41.13824298228534104, 76.23356602378127889 ) ) ;
#15716 = CARTESIAN_POINT ( 'NONE',  ( -7.347204055457580374, 41.85239250246546305, 77.69936312477425133 ) ) ;
#15717 = VERTEX_POINT ( 'NONE', #19213 ) ;
#15718 = CARTESIAN_POINT ( 'NONE',  ( 2.112264789766074458, 52.95437732364958094, 76.31288873172051979 ) ) ;
#15719 = ORIENTED_EDGE ( 'NONE', *, *, #4670, .F. ) ;
#15720 = AXIS2_PLACEMENT_3D ( 'NONE', #3993, #3679, #276 ) ;
#15721 = CARTESIAN_POINT ( 'NONE',  ( 6.154942347677927472, 50.94188193477284443, 75.39427037473855364 ) ) ;
#15722 = CARTESIAN_POINT ( 'NONE',  ( 4.722153740306518799, 44.16218137147969003, 56.15433879953099705 ) ) ;
#15723 = CARTESIAN_POINT ( 'NONE',  ( 5.568489401881125289, 48.03437091500646261, 91.82058880123797451 ) ) ;
#15724 = VECTOR ( 'NONE', #9273, 1000.000000000000227 ) ;
#15725 = DIRECTION ( 'NONE',  ( -0.000000000000000000, -0.000000000000000000, 1.000000000000000000 ) ) ;
#15726 = ORIENTED_EDGE ( 'NONE', *, *, #16614, .T. ) ;
#15727 = ORIENTED_EDGE ( 'NONE', *, *, #17314, .F. ) ;
#15728 = CARTESIAN_POINT ( 'NONE',  ( -3.763323997310421554, 36.38727654169121450, 75.66260743385902288 ) ) ;
#15729 = CARTESIAN_POINT ( 'NONE',  ( -5.208859716003345852, 50.02743738586465838, 75.74732467541012682 ) ) ;
#15730 = ORIENTED_EDGE ( 'NONE', *, *, #630, .T. ) ;
#15731 = CARTESIAN_POINT ( 'NONE',  ( -6.427915807670530945, 42.26053564693651055, 78.13669174070733447 ) ) ;
#15732 = DIRECTION ( 'NONE',  ( -0.9485903129789495791, 0.3165065846431928120, -8.934458285744765648E-17 ) ) ;
#15733 = CARTESIAN_POINT ( 'NONE',  ( 2.635245049009970142, 48.69372030666295359, 91.70433879953097289 ) ) ;
#15734 = EDGE_LOOP ( 'NONE', ( #2414, #7229, #13014, #8656 ) ) ;
#15735 = CARTESIAN_POINT ( 'NONE',  ( 5.424439005889565735, 37.58880062289685497, 77.71652930830589412 ) ) ;
#15736 = CARTESIAN_POINT ( 'NONE',  ( -6.711977078592299861, 40.31944429845940903, 78.72343487459158951 ) ) ;
#15737 = LINE ( 'NONE', #17626, #11911 ) ;
#15738 = CARTESIAN_POINT ( 'NONE',  ( -0.3080929418689875576, 37.85583172076933778, 92.60183880123797451 ) ) ;
#15739 = DIRECTION ( 'NONE',  ( -0.8043570849667761591, 0.5941461771851692664, -1.733862608106489734E-17 ) ) ;
#15740 = CIRCLE ( 'NONE', #12674, 9.999999999999996447 ) ;
#15741 = LINE ( 'NONE', #9144, #12261 ) ;
#15742 = EDGE_CURVE ( 'NONE', #4231, #11953, #20390, .T. ) ;
#15743 = AXIS2_PLACEMENT_3D ( 'NONE', #4774, #14369, #3200 ) ;
#15744 = CARTESIAN_POINT ( 'NONE',  ( 4.987494971863720927, 47.58855820898865829, 92.52371380294498238 ) ) ;
#15745 = ADVANCED_FACE ( 'NONE', ( #15618 ), #14115, .T. ) ;
#15746 = DIRECTION ( 'NONE',  ( -1.110223024625156540E-16, -1.000000000000000000, -5.922860397471808077E-17 ) ) ;
#15747 = CARTESIAN_POINT ( 'NONE',  ( 8.375217360078613282, 41.81485783204666262, 78.44085888008430629 ) ) ;
#15748 = DIRECTION ( 'NONE',  ( -4.731737692062791983E-17, 0.7071067811865500152, 0.7071067811865451302 ) ) ;
#15749 = DIRECTION ( 'NONE',  ( 1.540237394707284220E-16, 1.793354297423764243E-16, -1.000000000000000000 ) ) ;
#15750 = LINE ( 'NONE', #17334, #7196 ) ;
#15751 = CARTESIAN_POINT ( 'NONE',  ( 8.394097411062748648, 39.95136695475236621, 78.67376765716130649 ) ) ;
#15752 = LINE ( 'NONE', #1171, #2441 ) ;
#15753 = EDGE_CURVE ( 'NONE', #5246, #11086, #5929, .T. ) ;
#15754 = ADVANCED_FACE ( 'NONE', ( #5050 ), #168, .T. ) ;
#15755 = VECTOR ( 'NONE', #4968, 1000.000000000000000 ) ;
#15756 = CARTESIAN_POINT ( 'NONE',  ( 4.199109002476567376, 47.83913663364971569, 94.73786078214052964 ) ) ;
#15757 = DIRECTION ( 'NONE',  ( -2.838338907332122006E-16, 1.000000000000000000, 0.000000000000000000 ) ) ;
#15758 = ADVANCED_FACE ( 'NONE', ( #17729 ), #719, .T. ) ;
#15759 = ORIENTED_EDGE ( 'NONE', *, *, #529, .T. ) ;
#15760 = CARTESIAN_POINT ( 'NONE',  ( 8.255316794306208905, 41.43478779768023657, 78.91184774808348834 ) ) ;
#15761 = CARTESIAN_POINT ( 'NONE',  ( -4.189188114579791566, 36.70184521026505564, 79.48068319027247242 ) ) ;
#15762 = EDGE_CURVE ( 'NONE', #17246, #15617, #4401, .T. ) ;
#15763 = LINE ( 'NONE', #2771, #15724 ) ;
#15765 = ADVANCED_FACE ( 'NONE', ( #17497 ), #4936, .F. ) ;
#15764 = DIRECTION ( 'NONE',  ( -0.9534635866061452747, -0.3015081906286225522, -2.009271279954815797E-16 ) ) ;
#15766 = DIRECTION ( 'NONE',  ( -1.402518428993831183E-16, 1.000000000000000000, -3.469446951953617147E-16 ) ) ;
#15767 = CARTESIAN_POINT ( 'NONE',  ( -4.159599872275752119, 50.89444720483701445, 78.93089747760657815 ) ) ;
#15768 = DIRECTION ( 'NONE',  ( 0.4999999999999977240, -0.8660254037844398178, -0.000000000000000000 ) ) ;
#15769 = EDGE_CURVE ( 'NONE', #10737, #5474, #6410, .T. ) ;
#15770 = AXIS2_PLACEMENT_3D ( 'NONE', #1409, #15886, #6286 ) ;
#15771 = VERTEX_POINT ( 'NONE', #8234 ) ;
#15772 = CARTESIAN_POINT ( 'NONE',  ( -4.567115856812060670, 47.10047254335474065, 90.80496380123797451 ) ) ;
#15773 = PLANE ( 'NONE',  #8543 ) ;
#15774 = CARTESIAN_POINT ( 'NONE',  ( 5.887048643069795695, 51.13976422295020541, 78.81551702238962775 ) ) ;
#15775 = DIRECTION ( 'NONE',  ( 1.540237394707284220E-16, 1.793354297423764243E-16, -1.000000000000000000 ) ) ;
#15776 = ORIENTED_EDGE ( 'NONE', *, *, #2434, .F. ) ;
#15777 = DIRECTION ( 'NONE',  ( -0.5941461771851693774, -0.8043570849667760481, -2.357623395011396791E-16 ) ) ;
#15778 = CARTESIAN_POINT ( 'NONE',  ( -2.904223097202481174, 48.62752260303690122, 90.33621380294496817 ) ) ;
#15779 = EDGE_LOOP ( 'NONE', ( #3742, #15809, #7723, #621 ) ) ;
#15780 = DIRECTION ( 'NONE',  ( -1.540237394707284220E-16, -1.793354297423764243E-16, 1.000000000000000000 ) ) ;
#15781 = VECTOR ( 'NONE', #20793, 1000.000000000000227 ) ;
#15782 = CARTESIAN_POINT ( 'NONE',  ( 2.421193248165596668, 49.85372324935340060, 82.45433879953087342 ) ) ;
#15783 = CARTESIAN_POINT ( 'NONE',  ( -4.286600153180515349, 50.80436647093155500, 75.97348986337627252 ) ) ;
#15784 = DIRECTION ( 'NONE',  ( 1.000000000000000000, 0.000000000000000000, 0.000000000000000000 ) ) ;
#15785 = CARTESIAN_POINT ( 'NONE',  ( 0.8418751258662160453, 52.35219190451967108, 76.22640136859038762 ) ) ;
#15786 = EDGE_CURVE ( 'NONE', #4554, #14081, #19990, .T. ) ;
#15787 = CARTESIAN_POINT ( 'NONE',  ( -3.244219893606751892, 36.91785025630225192, 79.10742496273583413 ) ) ;
#15788 = VERTEX_POINT ( 'NONE', #14722 ) ;
#15789 = DIRECTION ( 'NONE',  ( -1.110223024625156540E-16, -1.000000000000000000, -5.922860397471808077E-17 ) ) ;
#15790 = ORIENTED_EDGE ( 'NONE', *, *, #5756, .T. ) ;
#15791 = CARTESIAN_POINT ( 'NONE',  ( 6.260406454228516715, 50.01997504955222240, 77.76256480524379811 ) ) ;
#15792 = CARTESIAN_POINT ( 'NONE',  ( 25.03948732994508219, 43.16218137147969003, 74.70433879953100131 ) ) ;
#15793 = CARTESIAN_POINT ( 'NONE',  ( -2.416137431568557314, 39.07291177436112406, 96.11746380123797451 ) ) ;
#15794 = DIRECTION ( 'NONE',  ( 0.3165065846431826535, 0.9485903129789529098, 2.188653791613874008E-16 ) ) ;
#15795 = CARTESIAN_POINT ( 'NONE',  ( -4.168645781477386514, 37.43637816616016067, 78.16907664373232478 ) ) ;
#15796 = PLANE ( 'NONE',  #17067 ) ;
#15797 = ORIENTED_EDGE ( 'NONE', *, *, #11706, .F. ) ;
#15798 = DIRECTION ( 'NONE',  ( 1.540237394707284220E-16, 1.793354297423764243E-16, -1.000000000000000000 ) ) ;
#15799 = ORIENTED_EDGE ( 'NONE', *, *, #19135, .T. ) ;
#15800 = CARTESIAN_POINT ( 'NONE',  ( -2.949171347157247602, 51.57769619255444837, 76.19075138459079710 ) ) ;
#15801 = CARTESIAN_POINT ( 'NONE',  ( -4.524181921268124462, 40.28999182795290324, 96.19558880123798872 ) ) ;
#15802 = DIRECTION ( 'NONE',  ( 1.540237394707284220E-16, 1.793354297423764243E-16, -1.000000000000000000 ) ) ;
#15803 = VERTEX_POINT ( 'NONE', #142 ) ;
#15804 = CARTESIAN_POINT ( 'NONE',  ( -4.574316323987746458, 51.33620267474496757, 79.54845644658969661 ) ) ;
#15805 = CARTESIAN_POINT ( 'NONE',  ( 5.053692675489762642, 42.04909006277621586, 93.57933879611698558 ) ) ;
#15806 = ORIENTED_EDGE ( 'NONE', *, *, #6047, .T. ) ;
#15807 = CARTESIAN_POINT ( 'NONE',  ( -4.165371047737147947, 37.43888844440124331, 78.75608284215286403 ) ) ;
#15808 = CARTESIAN_POINT ( 'NONE',  ( -4.451527680475927617, 51.42394294381934117, 78.89116106075270807 ) ) ;
#15809 = ORIENTED_EDGE ( 'NONE', *, *, #5185, .T. ) ;
#15810 = DIRECTION ( 'NONE',  ( -0.3165065846431827645, -0.9485903129789529098, 0.000000000000000000 ) ) ;
#15811 = CARTESIAN_POINT ( 'NONE',  ( 0.7139826536211262287, 52.35321313159215606, 78.90093525964157095 ) ) ;
#15812 = ORIENTED_EDGE ( 'NONE', *, *, #10424, .F. ) ;
#15813 = CARTESIAN_POINT ( 'NONE',  ( -4.554812065480294159, 50.60227710243181320, 79.52115730712957031 ) ) ;
#15814 = CARTESIAN_POINT ( 'NONE',  ( 5.248154646208118557, 37.46097559620424278, 75.97540876731110870 ) ) ;
#15815 = B_SPLINE_CURVE_WITH_KNOTS ( 'NONE', 3,
 ( #2269, #18445, #15150, #3750, #2171, #10383, #16852, #20130, #5567, #18550, #3963, #17373 ),
 .UNSPECIFIED., .F., .F.,
 ( 4, 2, 2, 2, 2, 4 ),
 ( 0.000000000000000000, 9.318763199797678004E-05, 0.0001863752639959535601, 0.0002795628959939303266, 0.0003727505279919071201, 0.0007455010559837727153 ),
 .UNSPECIFIED. ) ;
#15816 = CARTESIAN_POINT ( 'NONE',  ( -1.419351766502866541, 49.49642391118513274, 91.15746379782397923 ) ) ;
#15817 = CARTESIAN_POINT ( 'NONE',  ( 5.074967109082280103, 37.34659833035915710, 76.61095391776262886 ) ) ;
#15818 = CARTESIAN_POINT ( 'NONE',  ( 5.649834628789608182, 51.31498465973561451, 78.90029747732744170 ) ) ;
#15819 = FACE_OUTER_BOUND ( 'NONE', #15587, .T. ) ;
#15820 = ORIENTED_EDGE ( 'NONE', *, *, #12458, .F. ) ;
#15821 = CARTESIAN_POINT ( 'NONE',  ( 2.118024385280204314, 52.95416971904506909, 78.36218633565054859 ) ) ;
#15822 = DIRECTION ( 'NONE',  ( 3.893792155548169402E-16, 7.183611964723547524E-17, -1.000000000000000000 ) ) ;
#15823 = ORIENTED_EDGE ( 'NONE', *, *, #8850, .F. ) ;
#15824 = CARTESIAN_POINT ( 'NONE',  ( 5.939900590116411472, 51.10072461867315496, 76.38301527011910252 ) ) ;
#15825 = DIRECTION ( 'NONE',  ( -1.540237394707284467E-16, -1.793354297423764243E-16, 1.000000000000000000 ) ) ;
#15826 = CARTESIAN_POINT ( 'NONE',  ( -5.154188915835984375, 42.64120994080404614, 95.96121380123798872 ) ) ;
#15827 = CARTESIAN_POINT ( 'NONE',  ( -2.918060694704116553, 51.60562986935836705, 76.59715360994732691 ) ) ;
#15828 = ORIENTED_EDGE ( 'NONE', *, *, #3240, .F. ) ;
#15829 = VERTEX_POINT ( 'NONE', #19601 ) ;
#15830 = CARTESIAN_POINT ( 'NONE',  ( -4.412760631825748625, 36.86698922270429790, 75.37821288891845484 ) ) ;
#15831 = CARTESIAN_POINT ( 'NONE',  ( -6.776146237002087069, 40.42343150244711580, 77.93113452919423878 ) ) ;
#15832 = ORIENTED_EDGE ( 'NONE', *, *, #11078, .T. ) ;
#15833 = LINE ( 'NONE', #20392, #9461 ) ;
#15834 =( BOUNDED_CURVE ( )  B_SPLINE_CURVE ( 3, ( #10977, #15855, #19046, #12663 ),
 .UNSPECIFIED., .F., .F. ) 
 B_SPLINE_CURVE_WITH_KNOTS ( ( 4, 4 ),
 ( 1.982313172862381956, 2.094395102393196595 ),
 .UNSPECIFIED. ) 
 CURVE ( )  GEOMETRIC_REPRESENTATION_ITEM ( )  RATIONAL_B_SPLINE_CURVE ( ( 1.000000000000000000, 0.9989534107080366709, 0.9989534107080366709, 1.000000000000000000 ) ) 
 REPRESENTATION_ITEM ( '' )  );
#15835 = CARTESIAN_POINT ( 'NONE',  ( -6.888911687209406942, 40.65211947644671397, 79.25535243502660876 ) ) ;
#15836 = CARTESIAN_POINT ( 'NONE',  ( 8.390845173051939554, 39.94161979111582639, 76.38443001783366526 ) ) ;
#15837 = VERTEX_POINT ( 'NONE', #20976 ) ;
#15838 = CARTESIAN_POINT ( 'NONE',  ( 6.462272072047026583, 49.81511955649013146, 75.97564824412397400 ) ) ;
#15839 = CARTESIAN_POINT ( 'NONE',  ( 5.785641543149844246, 51.21466956273390991, 77.95070864408322109 ) ) ;
#15840 = CARTESIAN_POINT ( 'NONE',  ( 6.440194062841372968, 38.48619335307391509, 76.30003524316248331 ) ) ;
#15841 = CARTESIAN_POINT ( 'NONE',  ( 4.394343283833276992, 39.11584570990505938, 92.75808880123797451 ) ) ;
#15842 = ADVANCED_FACE ( 'NONE', ( #9530 ), #8643, .T. ) ;
#15843 = CARTESIAN_POINT ( 'NONE',  ( 8.616653853821931719, 45.47331367307960193, 79.47125056423675460 ) ) ;
#15844 = CARTESIAN_POINT ( 'NONE',  ( -7.297414422513008425, 40.12555000982377607, 78.68345068850670998 ) ) ;
#15845 = DIRECTION ( 'NONE',  ( 0.007885122365275663500, 0.9999689119394085113, 1.805443505845543142E-16 ) ) ;
#15846 = CARTESIAN_POINT ( 'NONE',  ( 30.92220646078100188, 45.56218137147968861, 62.80715055817104542 ) ) ;
#15847 = CARTESIAN_POINT ( 'NONE',  ( -1.348357406114881529, 47.70104341108812918, 77.28382765310962554 ) ) ;
#15848 = CARTESIAN_POINT ( 'NONE',  ( 29.77115333998617785, 40.36218137147969287, 105.5543387995309956 ) ) ;
#15849 = CARTESIAN_POINT ( 'NONE',  ( 8.638826686988997139, 40.68483612003910110, 79.45050910333212357 ) ) ;
#15850 = VERTEX_POINT ( 'NONE', #5023 ) ;
#15851 = CARTESIAN_POINT ( 'NONE',  ( -7.584911022892848464, 43.05104850827407148, 78.89751519991851580 ) ) ;
#15852 = CARTESIAN_POINT ( 'NONE',  ( 5.658108625003792191, 37.01637447524286273, 75.97198585835440099 ) ) ;
#15853 = EDGE_CURVE ( 'NONE', #17396, #18944, #10774, .T. ) ;
#15854 = VERTEX_POINT ( 'NONE', #4704 ) ;
#15855 = CARTESIAN_POINT ( 'NONE',  ( -1.214884381343041664, 47.76843358786783966, 69.41730067788145675 ) ) ;
#15856 = CARTESIAN_POINT ( 'NONE',  ( 1.514255888186003762, 51.36218137147968577, 83.03825919817350609 ) ) ;
#15857 = CARTESIAN_POINT ( 'NONE',  ( 2.522153740306509739, 47.62628298661744708, 58.55433879953100984 ) ) ;
#15858 = DIRECTION ( 'NONE',  ( -0.7938652969193448206, 0.6080936526121289987, -1.322136515275012895E-17 ) ) ;
#15859 = CARTESIAN_POINT ( 'NONE',  ( 5.627315617218822119, 51.33161854646183997, 78.02054163389647101 ) ) ;
#15860 = CARTESIAN_POINT ( 'NONE',  ( -4.032527917761953518, 50.98089643325306497, 78.50425692432636993 ) ) ;
#15861 = DIRECTION ( 'NONE',  ( -1.000000000000000000, 0.000000000000000000, -1.196361017915039239E-16 ) ) ;
#15862 = DIRECTION ( 'NONE',  ( -5.968085353131216186E-17, -0.4999999999999999445, -0.8660254037844387076 ) ) ;
#15863 = ADVANCED_FACE ( 'NONE', ( #11232 ), #3132, .T. ) ;
#15864 = ADVANCED_FACE ( 'NONE', ( #17703 ), #1755, .T. ) ;
#15865 = VECTOR ( 'NONE', #6808, 999.9999999999998863 ) ;
#15866 = ORIENTED_EDGE ( 'NONE', *, *, #5047, .T. ) ;
#15867 = CARTESIAN_POINT ( 'NONE',  ( 3.460444912181559474, 49.25145096859824889, 90.49246380123798872 ) ) ;
#15868 = LINE ( 'NONE', #6170, #4109 ) ;
#15869 = EDGE_CURVE ( 'NONE', #19551, #1329, #3332, .T. ) ;
#15870 = CARTESIAN_POINT ( 'NONE',  ( 5.254337203439246373, 50.85892981167459936, 78.80131646080216967 ) ) ;
#15871 = EDGE_LOOP ( 'NONE', ( #2274, #6744, #12057, #8495 ) ) ;
#15872 = DIRECTION ( 'NONE',  ( -0.4999999999999983347, -0.8660254037844395958, -0.000000000000000000 ) ) ;
#15873 = CARTESIAN_POINT ( 'NONE',  ( 4.987494971863720927, 47.58855820898865829, 90.02371380294498238 ) ) ;
#15874 = ORIENTED_EDGE ( 'NONE', *, *, #1162, .T. ) ;
#15875 = CARTESIAN_POINT ( 'NONE',  ( 5.493694769708608483, 50.67720340734032902, 78.89719962956496602 ) ) ;
#15876 = CARTESIAN_POINT ( 'NONE',  ( -0.9244181309328289853, 52.21935397360262954, 76.32609705745309725 ) ) ;
#15877 = VECTOR ( 'NONE', #20015, 1000.000000000000000 ) ;
#15878 = CARTESIAN_POINT ( 'NONE',  ( 4.772654808018759631, 51.96292205838052070, 79.19424447893550223 ) ) ;
#15879 = CARTESIAN_POINT ( 'NONE',  ( 5.385255718775495026, 47.76702405936703855, 72.45433879953087342 ) ) ;
#15880 = CARTESIAN_POINT ( 'NONE',  ( 26.43948732994508788, 43.16218137147969003, 76.90433879953101837 ) ) ;
#15881 = CARTESIAN_POINT ( 'NONE',  ( 30.92220646078100188, 42.76218137147968434, 57.80715055817105252 ) ) ;
#15882 = ORIENTED_EDGE ( 'NONE', *, *, #11078, .F. ) ;
#15883 = CARTESIAN_POINT ( 'NONE',  ( -5.368445182934975968, 51.36218137147968577, 53.35433879953099989 ) ) ;
#15884 = EDGE_LOOP ( 'NONE', ( #14355, #12890, #18502, #12687 ) ) ;
#15885 = CARTESIAN_POINT ( 'NONE',  ( 1.352400422481993658, 50.46853102219002096, 94.32058880123798872 ) ) ;
#15886 = DIRECTION ( 'NONE',  ( 0.000000000000000000, 0.000000000000000000, 1.000000000000000000 ) ) ;
#15887 = CARTESIAN_POINT ( 'NONE',  ( 0.5221537403065010796, 44.16218137147968292, 78.79551527011911105 ) ) ;
#15888 = DIRECTION ( 'NONE',  ( -0.5813877811927012917, 0.8136266022444372803, 5.636455622144620416E-17 ) ) ;
#15889 = EDGE_CURVE ( 'NONE', #12110, #14806, #16217, .T. ) ;
#15890 = FACE_OUTER_BOUND ( 'NONE', #5695, .T. ) ;
#15891 = AXIS2_PLACEMENT_3D ( 'NONE', #16269, #1700, #20925 ) ;
#15892 = ORIENTED_EDGE ( 'NONE', *, *, #647, .F. ) ;
#15893 = EDGE_CURVE ( 'NONE', #15145, #13051, #14038, .T. ) ;
#15894 = DIRECTION ( 'NONE',  ( 0.3165065846431827090, 0.9485903129789529098, 2.188653791613874994E-16 ) ) ;
#15895 = ADVANCED_FACE ( 'NONE', ( #7919 ), #12919, .T. ) ;
#15896 = EDGE_CURVE ( 'NONE', #18875, #1268, #11437, .T. ) ;
#15897 = ORIENTED_EDGE ( 'NONE', *, *, #17932, .F. ) ;
#15898 = CARTESIAN_POINT ( 'NONE',  ( -3.555031842569258416, 52.06454604677990972, 75.79042024895623797 ) ) ;
#15899 = CARTESIAN_POINT ( 'NONE',  ( -0.3080929418689875576, 37.85583172076933778, 92.60183880123797451 ) ) ;
#15900 = CARTESIAN_POINT ( 'NONE',  ( 8.617838889373357958, 45.46597658821364263, 78.74919174070734584 ) ) ;
#15901 = EDGE_LOOP ( 'NONE', ( #5490, #13404, #17152, #7639, #3056, #3297, #4831, #16374 ) ) ;
#15902 = CARTESIAN_POINT ( 'NONE',  ( -5.134596719205594795, 50.01589981793483020, 79.19259575086972802 ) ) ;
#15903 = DIRECTION ( 'NONE',  ( -0.9485903129789527988, 0.3165065846431829311, -8.934458285744989980E-17 ) ) ;
#15904 = VECTOR ( 'NONE', #9905, 1000.000000000000000 ) ;
#15905 = CARTESIAN_POINT ( 'NONE',  ( 6.388813065772197319, 37.53850911581889704, 78.31663032931759005 ) ) ;
#15906 = CARTESIAN_POINT ( 'NONE',  ( 5.202764418357927134, 50.89058147309204827, 76.27120023672567584 ) ) ;
#15907 = ORIENTED_EDGE ( 'NONE', *, *, #7879, .F. ) ;
#15908 = DIRECTION ( 'NONE',  ( -1.000000000000000000, -3.942553354492745503E-16, -0.000000000000000000 ) ) ;
#15909 = CARTESIAN_POINT ( 'NONE',  ( -3.350035803220276609, 49.20851703305431357, 92.13308880123798872 ) ) ;
#15910 = AXIS2_PLACEMENT_3D ( 'NONE', #20696, #18908, #7312 ) ;
#15911 = ORIENTED_EDGE ( 'NONE', *, *, #2635, .F. ) ;
#15912 = CARTESIAN_POINT ( 'NONE',  ( 10.77494014480653561, 42.76218137147968434, 74.20433879953100131 ) ) ;
#15913 = PLANE ( 'NONE',  #13595 ) ;
#15914 = CARTESIAN_POINT ( 'NONE',  ( -4.812088799398940075, 42.22067586467031930, 95.21996379782397923 ) ) ;
#15915 = CARTESIAN_POINT ( 'NONE',  ( 0.3869120917952212912, 35.96329670974014192, 76.16022115247204738 ) ) ;
#15916 = CARTESIAN_POINT ( 'NONE',  ( 0.5221537403065005245, 44.16218137147968292, 82.45433879953087342 ) ) ;
#15917 = VECTOR ( 'NONE', #15768, 1000.000000000000114 ) ;
#15918 = CARTESIAN_POINT ( 'NONE',  ( 5.939862031672385356, 51.10075310024252815, 76.36217657474753651 ) ) ;
#15919 = VERTEX_POINT ( 'NONE', #639 ) ;
#15920 = EDGE_CURVE ( 'NONE', #20386, #5547, #20099, .T. ) ;
#15921 = CARTESIAN_POINT ( 'NONE',  ( -6.946982443395988582, 47.54813533618698074, 78.32326721260994873 ) ) ;
#15922 = LINE ( 'NONE', #17607, #6581 ) ;
#15923 = ORIENTED_EDGE ( 'NONE', *, *, #9548, .T. ) ;
#15924 = CARTESIAN_POINT ( 'NONE',  ( 2.232254456934871900, 39.46371826755015633, 92.48558879953097289 ) ) ;
#15925 = CARTESIAN_POINT ( 'NONE',  ( 0.4729534506053946763, 52.36291882769025818, 75.36214536511981521 ) ) ;
#15926 = PLANE ( 'NONE',  #2788 ) ;
#15927 = DIRECTION ( 'NONE',  ( -5.626130192357176673E-16, -1.831515347669941892E-30, 1.000000000000000000 ) ) ;
#15928 = ORIENTED_EDGE ( 'NONE', *, *, #19210, .F. ) ;
#15929 = DIRECTION ( 'NONE',  ( -1.000000000000000000, 1.110223024625156540E-16, -1.779391786395883043E-16 ) ) ;
#15930 = ORIENTED_EDGE ( 'NONE', *, *, #14059, .T. ) ;
#15931 = CARTESIAN_POINT ( 'NONE',  ( -3.716790732209381165, 36.35290429323532635, 75.71473766112499959 ) ) ;
#15932 = CARTESIAN_POINT ( 'NONE',  ( -5.405939962049822078, 49.82766502745145942, 72.45433879953087342 ) ) ;
#15933 = CARTESIAN_POINT ( 'NONE',  ( 5.461659944059998217, 50.53996671397857909, 79.54598470662274678 ) ) ;
#15934 = VERTEX_POINT ( 'NONE', #17030 ) ;
#15935 = CARTESIAN_POINT ( 'NONE',  ( -4.529824687616612167, 37.72822084386444885, 77.32461911834714385 ) ) ;
#15936 = CARTESIAN_POINT ( 'NONE',  ( 8.211795273144437246, 41.32505156136733149, 77.24417474779077963 ) ) ;
#15937 = AXIS2_PLACEMENT_3D ( 'NONE', #13862, #9200, #15794 ) ;
#15938 = EDGE_LOOP ( 'NONE', ( #4103, #6194, #44, #16422, #20264 ) ) ;
#15939 = CARTESIAN_POINT ( 'NONE',  ( 5.497232476171135751, 37.64385397974522363, 77.42016051845197921 ) ) ;
#15940 = CARTESIAN_POINT ( 'NONE',  ( 5.901631269491789844, 51.12899262423628954, 78.24916896818955081 ) ) ;
#15941 = CARTESIAN_POINT ( 'NONE',  ( 2.263811127080450625, 49.90383875825364157, 85.41268141275705261 ) ) ;
#15942 = CARTESIAN_POINT ( 'NONE',  ( -0.3080929418689875576, 37.85583172076933778, 91.35183880123798872 ) ) ;
#15943 = SHAPE_REPRESENTATION_RELATIONSHIP ( 'NONE' , 'NONE' ,  #7678, #9085 ) ;
#15944 = EDGE_CURVE ( 'NONE', #1872, #9681, #5422, .T. ) ;
#15945 = CARTESIAN_POINT ( 'NONE',  ( 5.787513446439723985, 51.21328686317854562, 75.36061482756318242 ) ) ;
#15946 = CARTESIAN_POINT ( 'NONE',  ( -0.1709386726045586946, 50.28109722957945138, 83.67325465763076409 ) ) ;
#15947 = DIRECTION ( 'NONE',  ( -0.3165065846431826535, -0.9485903129789529098, -2.188653791613874008E-16 ) ) ;
#15948 = VECTOR ( 'NONE', #5013, 1000.000000000000000 ) ;
#15949 = CARTESIAN_POINT ( 'NONE',  ( -0.4845124703328578253, 52.97630383655213393, 79.30111418114536548 ) ) ;
#15950 = ORIENTED_EDGE ( 'NONE', *, *, #18874, .F. ) ;
#15951 = DIRECTION ( 'NONE',  ( 0.000000000000000000, 0.000000000000000000, 1.000000000000000000 ) ) ;
#15952 = PLANE ( 'NONE',  #11971 ) ;
#15953 = CARTESIAN_POINT ( 'NONE',  ( 8.557023814081752278, 40.43966772045860125, 79.34450935619591405 ) ) ;
#15954 = FILL_AREA_STYLE ('',( #18720 ) ) ;
#15955 =( BOUNDED_CURVE ( )  B_SPLINE_CURVE ( 2, ( #1813, #1492, #1596, #18079, #17863, #8396, #3498, #10008, #14876, #14775, #13186, #19660, #19346, #297, #19557, #6472, #4977 ),
 .UNSPECIFIED., .F., .F. ) 
 B_SPLINE_CURVE_WITH_KNOTS ( ( 3, 2, 2, 2, 2, 2, 2, 2, 3 ),
 ( 0.3050440133814064092, 0.3124899283300235364, 0.3385307556908612181, 0.3645715830516987888, 0.3906124104125364149, 0.4166532377733740411, 0.4426940651342116118, 0.4687348924950492934, 0.4934533006542767275 ),
 .UNSPECIFIED. ) 
 CURVE ( )  GEOMETRIC_REPRESENTATION_ITEM ( )  RATIONAL_B_SPLINE_CURVE ( ( 0.9689162008616551969, 0.9782346958905645540, 1.000000000000000000, 0.9238795325112867385, 1.000000000000000000, 0.9238795325112867385, 1.000000000000000000, 0.9238795325112867385, 1.000000000000000000, 0.9238795325112867385, 1.000000000000000000, 0.9238795325112867385, 1.000000000000000000, 0.9238795325112867385, 1.000000000000000000, 0.9277451227418798130, 0.9926614284736728910 ) ) 
 REPRESENTATION_ITEM ( '' )  );
#15956 = ORIENTED_EDGE ( 'NONE', *, *, #16758, .F. ) ;
#15957 = ORIENTED_EDGE ( 'NONE', *, *, #15051, .T. ) ;
#15958 = EDGE_CURVE ( 'NONE', #20749, #5251, #5856, .T. ) ;
#15959 = CARTESIAN_POINT ( 'NONE',  ( 8.161249387665455046, 41.17249610787522585, 75.37807442913842237 ) ) ;
#15960 = CARTESIAN_POINT ( 'NONE',  ( -3.535132420242971474, 36.21872061582891433, 78.58910375170351870 ) ) ;
#15961 = CARTESIAN_POINT ( 'NONE',  ( -4.873991315592629547, 37.20768174929764882, 78.81125587425833601 ) ) ;
#15962 = CARTESIAN_POINT ( 'NONE',  ( -3.638881865644721270, 47.35505628986900462, 93.82700776475003579 ) ) ;
#15963 = PLANE ( 'NONE',  #12167 ) ;
#15964 = AXIS2_PLACEMENT_3D ( 'NONE', #9619, #20565, #4493 ) ;
#15965 = CARTESIAN_POINT ( 'NONE',  ( 6.737194059699555204, 50.51179604963209613, 77.55733179791843668 ) ) ;
#15966 = DIRECTION ( 'NONE',  ( 1.193617070626243484E-16, 1.000000000000000000, 0.000000000000000000 ) ) ;
#15967 = CARTESIAN_POINT ( 'NONE',  ( 11.22215374030650281, 42.96218137147968008, 69.40574467885102194 ) ) ;
#15968 = VECTOR ( 'NONE', #5811, 1000.000000000000114 ) ;
#15969 = EDGE_CURVE ( 'NONE', #15210, #5897, #17137, .T. ) ;
#15970 = VERTEX_POINT ( 'NONE', #2559 ) ;
#15971 = DIRECTION ( 'NONE',  ( -1.779391786395883536E-16, -5.922860397471806844E-17, 1.000000000000000000 ) ) ;
#15972 = FACE_OUTER_BOUND ( 'NONE', #16986, .T. ) ;
#15973 = FACE_OUTER_BOUND ( 'NONE', #20419, .T. ) ;
#15974 = AXIS2_PLACEMENT_3D ( 'NONE', #6555, #1789, #19740 ) ;
#15975 = VECTOR ( 'NONE', #793, 1000.000000000000000 ) ;
#15976 = VERTEX_POINT ( 'NONE', #9055 ) ;
#15977 = DIRECTION ( 'NONE',  ( 0.5941461771851728191, 0.8043570849667734945, 2.357623395011397284E-16 ) ) ;
#15978 = CARTESIAN_POINT ( 'NONE',  ( -2.904223097202481174, 48.62752260303690122, 94.08621380294496817 ) ) ;
#15979 = EDGE_LOOP ( 'NONE', ( #5604, #10387, #15163, #10545 ) ) ;
#15980 = CARTESIAN_POINT ( 'NONE',  ( -1.854173455793826308, 49.13976469971947125, 94.80877693069184886 ) ) ;
#15982 = VECTOR ( 'NONE', #1880, 1000.000000000000000 ) ;
#15981 = CARTESIAN_POINT ( 'NONE',  ( -0.7091505932202195606, 52.97684993034207679, 75.80943630940421940 ) ) ;
#15983 = CARTESIAN_POINT ( 'NONE',  ( 5.319542448682613944, 51.55895818820005871, 79.51138782552760631 ) ) ;
#15984 = CARTESIAN_POINT ( 'NONE',  ( 5.309255083855641821, 37.50457964663987553, 75.97198585835440099 ) ) ;
#15985 = CARTESIAN_POINT ( 'NONE',  ( 2.037483459743116843, 49.33852326317117587, 92.45433879953093026 ) ) ;
#15986 = ORIENTED_EDGE ( 'NONE', *, *, #2645, .F. ) ;
#15987 = CARTESIAN_POINT ( 'NONE',  ( 8.296801588964658691, 41.57982088258064124, 75.97261045075327957 ) ) ;
#15988 = ORIENTED_EDGE ( 'NONE', *, *, #12169, .F. ) ;
#15989 = DIRECTION ( 'NONE',  ( 1.000000000000000000, 0.000000000000000000, 0.000000000000000000 ) ) ;
#15990 = LINE ( 'NONE', #6188, #5898 ) ;
#15991 = CARTESIAN_POINT ( 'NONE',  ( 1.116468592199672649, 52.94813999089376466, 76.77233108029956554 ) ) ;
#15992 = CARTESIAN_POINT ( 'NONE',  ( 2.522153740306509739, 49.16218137147969003, 58.55433879953100984 ) ) ;
#15993 = EDGE_CURVE ( 'NONE', #16819, #16316, #8845, .T. ) ;
#15994 = DIRECTION ( 'NONE',  ( -1.540237394707283727E-16, -1.793354297423763257E-16, 1.000000000000000000 ) ) ;
#15995 = B_SPLINE_SURFACE_WITH_KNOTS ( 'NONE', 3, 1, ( 
 ( #6561, #9679 ),
 ( #1580, #7752 ),
 ( #8061, #14230 ),
 ( #1889, #13168 ),
 ( #5166, #9884 ),
 ( #14759, #18163 ),
 ( #5375, #11477 ),
 ( #13379, #16364 ),
 ( #277, #11585 ),
 ( #18260, #5067 ),
 ( #1795, #11785 ),
 ( #3580, #3368 ),
 ( #8377, #18058 ),
 ( #8277, #2100 ),
 ( #19849, #8601 ),
 ( #3478, #17954 ),
 ( #11686, #181 ),
 ( #6664, #6766 ),
 ( #19642, #9990 ),
 ( #16469, #3680 ),
 ( #14860, #16782 ),
 ( #13277, #19746 ),
 ( #18370, #10087 ),
 ( #16569, #15080 ),
 ( #10197, #19946 ),
 ( #15180, #13577 ),
 ( #1991, #16677 ) ),
 .UNSPECIFIED., .F., .F., .F.,
 ( 4, 1, 1, 1, 1, 1, 1, 1, 1, 1, 1, 1, 1, 1, 1, 1, 1, 1, 1, 1, 1, 1, 1, 1, 4 ),
 ( 2, 2 ),
 ( 0.000000000000000000, 0.04992685941337848821, 0.09871136507264777205, 0.1457954968408328167, 0.1915776562037285746, 0.2364429891513756543, 0.2798905081306632403, 0.3226114784840122263, 0.3640369619956516645, 0.4040931382756795531, 0.4423864865660626644, 0.4791244981183566676, 0.5145420102664520767, 0.5484747442263178119, 0.5814193454185596632, 0.6141157465626525536, 0.6462545211269067336, 0.6795390940691592441, 0.7156628256359011120, 0.7545220547839790459, 0.7966562418723396322, 0.8423152836035615598, 0.8912945236129800053, 0.9437207944264596193, 1.000000000000000000 ),
 ( 0.000000000000000000, 1.000000000000000000 ),
 .UNSPECIFIED. ) ;
#15996 = AXIS2_PLACEMENT_3D ( 'NONE', #4360, #14153, #15977 ) ;
#15997 = VERTEX_POINT ( 'NONE', #18623 ) ;
#15998 = DIRECTION ( 'NONE',  ( -0.3165065846431825980, -0.9485903129789527988, 0.000000000000000000 ) ) ;
#15999 = VERTEX_POINT ( 'NONE', #18521 ) ;
#16000 = CARTESIAN_POINT ( 'NONE',  ( 2.522153740306510183, 50.16218137147969713, 58.55433879953100984 ) ) ;
#16001 = CARTESIAN_POINT ( 'NONE',  ( -3.981178359372548492, 46.76218137147973408, 91.35183879953098085 ) ) ;
#16002 = PLANE ( 'NONE',  #13220 ) ;
#16003 = ORIENTED_EDGE ( 'NONE', *, *, #1080, .F. ) ;
#16004 = EDGE_CURVE ( 'NONE', #8220, #3959, #16430, .T. ) ;
#16005 = LINE ( 'NONE', #1530, #8940 ) ;
#16006 = LINE ( 'NONE', #1426, #14700 ) ;
#16007 = CARTESIAN_POINT ( 'NONE',  ( 4.464802119779007761, 36.16368133634887982, 76.05895398371444571 ) ) ;
#16008 = CARTESIAN_POINT ( 'NONE',  ( 5.201045719205120932, 50.89185100692279207, 76.32883089164610624 ) ) ;
#16009 = ADVANCED_FACE ( 'NONE', ( #15543 ), #961, .F. ) ;
#16010 = CARTESIAN_POINT ( 'NONE',  ( 2.263363662449363822, 49.77488197367694767, 93.19231768333818877 ) ) ;
#16011 = ORIENTED_EDGE ( 'NONE', *, *, #4425, .T. ) ;
#16012 = CARTESIAN_POINT ( 'NONE',  ( -4.927487955684009435, 43.24703606169091330, 92.55433879953093879 ) ) ;
#16013 = DIRECTION ( 'NONE',  ( -1.000000000000000000, 0.000000000000000000, 0.000000000000000000 ) ) ;
#16014 = EDGE_LOOP ( 'NONE', ( #13691, #7042, #8411, #13028 ) ) ;
#16015 = CARTESIAN_POINT ( 'NONE',  ( 3.294548648621552278, 48.45522119969754016, 95.05433879953096721 ) ) ;
#16016 = DIRECTION ( 'NONE',  ( 0.000000000000000000, 0.000000000000000000, 1.000000000000000000 ) ) ;
#16017 = EDGE_CURVE ( 'NONE', #1583, #2188, #5061, .T. ) ;
#16018 = EDGE_CURVE ( 'NONE', #5376, #4661, #15439, .T. ) ;
#16019 = CARTESIAN_POINT ( 'NONE',  ( -5.403286049735823049, 49.82407567696579065, 76.72345405564152543 ) ) ;
#16020 = CARTESIAN_POINT ( 'NONE',  ( 5.856396280011940014, 46.10368687828906076, 93.34496379782399345 ) ) ;
#16021 = FACE_OUTER_BOUND ( 'NONE', #9471, .T. ) ;
#16022 = VECTOR ( 'NONE', #15447, 1000.000000000000000 ) ;
#16023 = EDGE_CURVE ( 'NONE', #7289, #1035, #1485, .T. ) ;
#16024 = CARTESIAN_POINT ( 'NONE',  ( 0.5221537403065015237, 44.16218137147968292, 75.45433879953087342 ) ) ;
#16025 = CARTESIAN_POINT ( 'NONE',  ( -3.711266317373846046, 36.34882363053331744, 77.55767546204062057 ) ) ;
#16026 = EDGE_LOOP ( 'NONE', ( #16036, #4083, #10065, #6935 ) ) ;
#16027 = CARTESIAN_POINT ( 'NONE',  ( 2.075775165176096060, 52.95450286967243159, 78.81257284323012868 ) ) ;
#16028 = CARTESIAN_POINT ( 'NONE',  ( 4.100026115879673583, 51.54044873340893673, 76.58963291717793709 ) ) ;
#16029 = ORIENTED_EDGE ( 'NONE', *, *, #13078, .T. ) ;
#16030 = CARTESIAN_POINT ( 'NONE',  ( 29.63948732994508006, 45.16218137147968292, 74.70433879953100131 ) ) ;
#16031 = CARTESIAN_POINT ( 'NONE',  ( 5.470702040720124337, 37.62937602372697654, 77.62670008255557264 ) ) ;
#16032 = CARTESIAN_POINT ( 'NONE',  ( 8.886583547266173611, 41.42737914769194418, 79.54795956895829079 ) ) ;
#16033 = CARTESIAN_POINT ( 'NONE',  ( 8.685073573159321825, 40.82344097173932340, 79.49103220525971381 ) ) ;
#16034 = ORIENTED_EDGE ( 'NONE', *, *, #8138, .F. ) ;
#16035 = CARTESIAN_POINT ( 'NONE',  ( -8.192078482032012943, 42.93655631659661509, 78.28007409364852265 ) ) ;
#16036 = ORIENTED_EDGE ( 'NONE', *, *, #19690, .F. ) ;
#16037 = VECTOR ( 'NONE', #3152, 1000.000000000000000 ) ;
#16038 = DIRECTION ( 'NONE',  ( -1.402518428993831183E-16, 1.000000000000000000, -3.469446951953617147E-16 ) ) ;
#16039 = CARTESIAN_POINT ( 'NONE',  ( -4.537713647263720951, 36.95928698179384497, 76.12832907849806929 ) ) ;
#16040 = CARTESIAN_POINT ( 'NONE',  ( -6.710037999761452987, 40.29754613885109649, 78.44771795036322715 ) ) ;
#16041 = CIRCLE ( 'NONE', #14684, 6.999999999999999112 ) ;
#16042 = ORIENTED_EDGE ( 'NONE', *, *, #13656, .T. ) ;
#16043 = CARTESIAN_POINT ( 'NONE',  ( -4.770044440429790811, 37.13090037985040226, 77.30667006270941499 ) ) ;
#16044 = CARTESIAN_POINT ( 'NONE',  ( -4.702170908118536552, 37.85552605441999674, 77.90218689189877921 ) ) ;
#16045 = CARTESIAN_POINT ( 'NONE',  ( -4.884656273474451638, 44.39824779480852612, 94.59496379953098710 ) ) ;
#16046 = VERTEX_POINT ( 'NONE', #2242 ) ;
#16047 = LINE ( 'NONE', #1787, #9408 ) ;
#16048 = CARTESIAN_POINT ( 'NONE',  ( -4.971268510706558175, 38.07201989387243657, 79.49652848452727483 ) ) ;
#16049 = EDGE_CURVE ( 'NONE', #13175, #20173, #19637, .T. ) ;
#16050 = CARTESIAN_POINT ( 'NONE',  ( 5.568489401881125289, 48.03437091500646261, 93.07058880123797451 ) ) ;
#16051 = LINE ( 'NONE', #11161, #19821 ) ;
#16052 = AXIS2_PLACEMENT_3D ( 'NONE', #8375, #16053, #11377 ) ;
#16053 = DIRECTION ( 'NONE',  ( -1.540237394707283727E-16, -1.793354297423763257E-16, 1.000000000000000000 ) ) ;
#16054 = DIRECTION ( 'NONE',  ( 1.779391786395883536E-16, 5.922860397471805611E-17, -1.000000000000000000 ) ) ;
#16055 = VECTOR ( 'NONE', #7011, 1000.000000000000000 ) ;
#16056 = CARTESIAN_POINT ( 'NONE',  ( -0.9334096104468154742, 52.21740282451978743, 78.43306491891449639 ) ) ;
#16057 = ORIENTED_EDGE ( 'NONE', *, *, #14662, .T. ) ;
#16058 = CARTESIAN_POINT ( 'NONE',  ( -4.537099264183359182, 37.70896829297682729, 78.18375056423674607 ) ) ;
#16059 = CARTESIAN_POINT ( 'NONE',  ( -1.219056181836354558, 49.77488197367695477, 94.40612966814926210 ) ) ;
#16060 = CARTESIAN_POINT ( 'NONE',  ( 5.653389158101303380, 51.31235907211823388, 75.98863418974025308 ) ) ;
#16061 = CARTESIAN_POINT ( 'NONE',  ( 6.903329084842819263, 50.38907879888579089, 78.20944795639196911 ) ) ;
#16062 = ORIENTED_EDGE ( 'NONE', *, *, #4525, .T. ) ;
#16063 = ORIENTED_EDGE ( 'NONE', *, *, #763, .F. ) ;
#16064 = AXIS2_PLACEMENT_3D ( 'NONE', #18511, #5200, #13411 ) ;
#16065 = CARTESIAN_POINT ( 'NONE',  ( 9.296966826988569466, 42.65732387124978686, 75.81656704941096336 ) ) ;
#16066 = DIRECTION ( 'NONE',  ( 1.000000000000000000, 6.123233995736766036E-17, 0.000000000000000000 ) ) ;
#16067 = CARTESIAN_POINT ( 'NONE',  ( -1.477846259693493813, 50.16218137147969713, 74.55433879953100984 ) ) ;
#16068 = VECTOR ( 'NONE', #6677, 1000.000000000000000 ) ;
#16069 = DIRECTION ( 'NONE',  ( 4.142850521348543581E-16, -5.922860397471813007E-17, 1.000000000000000000 ) ) ;
#16070 = CARTESIAN_POINT ( 'NONE',  ( -3.944959226007137776, 38.51060946023304865, 78.18375056423674607 ) ) ;
#16071 = CARTESIAN_POINT ( 'NONE',  ( -3.184806123434658964, 36.84768901790411633, 75.88014116946466459 ) ) ;
#16072 = CARTESIAN_POINT ( 'NONE',  ( 8.551362112893849954, 42.78711729333979719, 77.91040118276930571 ) ) ;
#16073 = CARTESIAN_POINT ( 'NONE',  ( -1.769308508470985419, 51.40850462968639079, 72.45433879953087342 ) ) ;
#16074 = CARTESIAN_POINT ( 'NONE',  ( 6.519609470440952848, 49.74768407388893365, 76.59575135851817151 ) ) ;
#16075 = CARTESIAN_POINT ( 'NONE',  ( 25.63948732994508362, 36.35905713404684292, 76.90433879953101837 ) ) ;
#16076 = ADVANCED_FACE ( 'NONE', ( #8076 ), #17762, .T. ) ;
#16077 = CIRCLE ( 'NONE', #6888, 3.999999999999996447 ) ;
#16078 = FACE_OUTER_BOUND ( 'NONE', #7714, .T. ) ;
#16079 = CARTESIAN_POINT ( 'NONE',  ( -3.087839404999279225, 36.79949025498288506, 77.19021729766356543 ) ) ;
#16080 = ORIENTED_EDGE ( 'NONE', *, *, #2095, .F. ) ;
#16081 = CARTESIAN_POINT ( 'NONE',  ( 11.22215374030650281, 45.56218137147968861, 62.80715055817104542 ) ) ;
#16082 = FACE_OUTER_BOUND ( 'NONE', #12396, .T. ) ;
#16083 = VERTEX_POINT ( 'NONE', #18933 ) ;
#16084 = CARTESIAN_POINT ( 'NONE',  ( 6.866536783559561208, 37.87987299396810670, 76.25518385353585415 ) ) ;
#16085 = CARTESIAN_POINT ( 'NONE',  ( 4.833451453752482863, 51.91801402521529241, 79.26957207196610966 ) ) ;
#16086 = CARTESIAN_POINT ( 'NONE',  ( 11.22215374030650281, 51.36218137147968577, 54.55433879953099563 ) ) ;
#16087 = CARTESIAN_POINT ( 'NONE',  ( 0.8466962780023906676, 52.96359677974843549, 76.22640136859038762 ) ) ;
#16088 = CARTESIAN_POINT ( 'NONE',  ( 3.213865265001516480, 48.74132121123690808, 92.45433879953098710 ) ) ;
#16089 = VERTEX_POINT ( 'NONE', #14141 ) ;
#16090 = CARTESIAN_POINT ( 'NONE',  ( 5.848554534127551108, 37.15246014923294382, 77.40928489470421425 ) ) ;
#16091 = AXIS2_PLACEMENT_3D ( 'NONE', #19398, #8124, #1433 ) ;
#16092 = EDGE_LOOP ( 'NONE', ( #18317, #11795, #10266, #7134 ) ) ;
#16093 = CARTESIAN_POINT ( 'NONE',  ( 5.611423337425062385, 41.22389019960463230, 95.17996380123798872 ) ) ;
#16094 = CARTESIAN_POINT ( 'NONE',  ( -5.154188915835984375, 42.64120994080404614, 93.46121380123797451 ) ) ;
#16095 = DIRECTION ( 'NONE',  ( -0.3165065846431827645, -0.9485903129789529098, 0.000000000000000000 ) ) ;
#16096 = PLANE ( 'NONE',  #1167 ) ;
#16097 = CARTESIAN_POINT ( 'NONE',  ( -5.954976305145398108, 38.00616181634879354, 76.59693911441793546 ) ) ;
#16098 = ADVANCED_FACE ( 'NONE', ( #1595 ), #17451, .F. ) ;
#16099 = EDGE_CURVE ( 'NONE', #4999, #18556, #4348, .T. ) ;
#16100 = VERTEX_POINT ( 'NONE', #1272 ) ;
#16101 = CARTESIAN_POINT ( 'NONE',  ( 4.577225057937401864, 52.10727814237509392, 78.46169174070733732 ) ) ;
#16102 = VERTEX_POINT ( 'NONE', #2969 ) ;
#16103 = AXIS2_PLACEMENT_3D ( 'NONE', #4854, #19325, #12539 ) ;
#16104 = DIRECTION ( 'NONE',  ( 1.540237394707284220E-16, 1.793354297423764243E-16, -1.000000000000000000 ) ) ;
#16105 = CARTESIAN_POINT ( 'NONE',  ( 2.522153740306505298, 49.16218137147968292, 82.55433879953099563 ) ) ;
#16106 = CARTESIAN_POINT ( 'NONE',  ( 4.826069222465897646, 51.92346698209227895, 75.62563104034643402 ) ) ;
#16107 = ORIENTED_EDGE ( 'NONE', *, *, #12739, .F. ) ;
#16108 = CARTESIAN_POINT ( 'NONE',  ( 1.932239457924184167, 52.24021385314885180, 77.09260542632576119 ) ) ;
#16109 = CARTESIAN_POINT ( 'NONE',  ( -7.075244453723417593, 44.52209897503762193, 72.45432679953087529 ) ) ;
#16110 = CARTESIAN_POINT ( 'NONE',  ( 5.595869095536538218, 45.91955541653086925, 92.55433879953098142 ) ) ;
#16111 = ADVANCED_FACE ( 'NONE', ( #7663 ), #3189, .F. ) ;
#16112 = CARTESIAN_POINT ( 'NONE',  ( -1.579458713576543882, 38.67424504380988282, 95.05433879952670395 ) ) ;
#16113 = CYLINDRICAL_SURFACE ( 'NONE', #4800, 4.200000000000001954 ) ;
#16114 = ORIENTED_EDGE ( 'NONE', *, *, #19794, .F. ) ;
#16115 = LINE ( 'NONE', #11230, #11901 ) ;
#16116 = DIRECTION ( 'NONE',  ( -0.000000000000000000, 1.000000000000000000, 1.734723475976787531E-14 ) ) ;
#16117 = EDGE_CURVE ( 'NONE', #18186, #15405, #6238, .T. ) ;
#16118 = ORIENTED_EDGE ( 'NONE', *, *, #10699, .T. ) ;
#16119 = DIRECTION ( 'NONE',  ( 0.9485903129789529098, -0.3165065846431827090, 8.934458285744996143E-17 ) ) ;
#16120 = DIRECTION ( 'NONE',  ( 1.000000000000000000, 0.000000000000000000, 0.000000000000000000 ) ) ;
#16121 = CARTESIAN_POINT ( 'NONE',  ( 1.855487073639845885, 49.49551470481303284, 85.82100546619767556 ) ) ;
#16122 = CARTESIAN_POINT ( 'NONE',  ( 5.902048492000326441, 51.12868443877599134, 78.59183879953087626 ) ) ;
#16123 = CARTESIAN_POINT ( 'NONE',  ( 4.673174852049363004, 39.63213674411673537, 91.86058879782397923 ) ) ;
#16124 = CARTESIAN_POINT ( 'NONE',  ( -4.007890887056451135, 40.01116025973682611, 92.64183879782400766 ) ) ;
#16125 = EDGE_CURVE ( 'NONE', #5246, #14083, #4761, .T. ) ;
#16127 = EDGE_CURVE ( 'NONE', #5582, #19569, #7978, .T. ) ;
#16126 = DIRECTION ( 'NONE',  ( 0.3165065846431826535, 0.9485903129789529098, 2.188653791613874008E-16 ) ) ;
#16128 = EDGE_CURVE ( 'NONE', #14841, #12731, #18675, .T. ) ;
#16129 = CARTESIAN_POINT ( 'NONE',  ( -3.197219379186972521, 36.89395081135501897, 77.48323649892105891 ) ) ;
#16130 = ORIENTED_EDGE ( 'NONE', *, *, #17036, .T. ) ;
#16131 = CARTESIAN_POINT ( 'NONE',  ( 2.051935062045836311, 52.95469085764700878, 78.89969410769322167 ) ) ;
#16132 = CARTESIAN_POINT ( 'NONE',  ( -3.799282117832336603, 36.41383735683930212, 77.78682928037112276 ) ) ;
#16133 = PRODUCT_DEFINITION ( 'UNKNOWN', '', #706, #9980 ) ;
#16134 = ORIENTED_EDGE ( 'NONE', *, *, #18715, .F. ) ;
#16135 = DIRECTION ( 'NONE',  ( 6.308085367188358884E-15, 3.469446951953626515E-16, 1.000000000000000000 ) ) ;
#16136 = EDGE_CURVE ( 'NONE', #18561, #9638, #9694, .T. ) ;
#16137 = CARTESIAN_POINT ( 'NONE',  ( 31.03948732994507864, 45.16218137147969003, 76.90433879953100416 ) ) ;
#16138 = CARTESIAN_POINT ( 'NONE',  ( -2.938479363457391358, 51.59616431484483456, 76.29466226208309365 ) ) ;
#16139 = VERTEX_POINT ( 'NONE', #14245 ) ;
#16140 = FACE_OUTER_BOUND ( 'NONE', #19474, .T. ) ;
#16141 = EDGE_LOOP ( 'NONE', ( #6068, #9965, #15866, #12231 ) ) ;
#16142 = CARTESIAN_POINT ( 'NONE',  ( -7.932261308893451712, 41.72020721241317176, 78.84683602641649713 ) ) ;
#16143 = CARTESIAN_POINT ( 'NONE',  ( -4.165071384785050235, 37.43866709544969495, 76.22840587216694530 ) ) ;
#16144 = CARTESIAN_POINT ( 'NONE',  ( 3.122153740306552905, 48.66551347115873227, 93.53933879953099506 ) ) ;
#16145 = ORIENTED_EDGE ( 'NONE', *, *, #12606, .T. ) ;
#16146 = CARTESIAN_POINT ( 'NONE',  ( 4.578029447411149810, 52.10668397227361481, 78.50413411530853125 ) ) ;
#16147 = DIRECTION ( 'NONE',  ( 1.540237394707284220E-16, 1.793354297423764243E-16, -1.000000000000000000 ) ) ;
#16148 = CARTESIAN_POINT ( 'NONE',  ( 2.921181103050039418, 49.30691215337508737, 92.09496379782399345 ) ) ;
#16149 = ORIENTED_EDGE ( 'NONE', *, *, #389, .T. ) ;
#16150 = CARTESIAN_POINT ( 'NONE',  ( -4.774380534136511756, 51.19324411499089678, 76.08363728426196815 ) ) ;
#16151 = DIRECTION ( 'NONE',  ( 1.000000000000000000, 0.000000000000000000, 0.000000000000000000 ) ) ;
#16152 = CARTESIAN_POINT ( 'NONE',  ( 6.062689023816073330, 38.11643952539938596, 75.52723796482321461 ) ) ;
#16153 = CARTESIAN_POINT ( 'NONE',  ( 0.000000000000000000, 0.000000000000000000, 0.000000000000000000 ) ) ;
#16154 = CARTESIAN_POINT ( 'NONE',  ( -5.809877882140231264, 50.45331562208507847, 76.21531548689122815 ) ) ;
#16155 = CARTESIAN_POINT ( 'NONE',  ( 0.5221537403065019678, 44.16218137147968292, 72.45433879953087342 ) ) ;
#16156 = EDGE_CURVE ( 'NONE', #17907, #17272, #14361, .T. ) ;
#16157 = DIRECTION ( 'NONE',  ( -1.110223024625156540E-16, -1.000000000000000000, -5.922860397471808077E-17 ) ) ;
#16158 = PLANE ( 'NONE',  #3700 ) ;
#16159 = EDGE_LOOP ( 'NONE', ( #3033, #1036, #4635, #19055 ) ) ;
#16160 = FACE_OUTER_BOUND ( 'NONE', #16259, .T. ) ;
#16161 = DIRECTION ( 'NONE',  ( 0.000000000000000000, 0.000000000000000000, -1.000000000000000000 ) ) ;
#16162 = EDGE_CURVE ( 'NONE', #5158, #20921, #14569, .T. ) ;
#16163 = CARTESIAN_POINT ( 'NONE',  ( 8.872773925109784798, 41.38599083402314704, 79.54845644658969661 ) ) ;
#16164 = CARTESIAN_POINT ( 'NONE',  ( 0.8435675618935688513, 52.95685645435612088, 79.54466172167512639 ) ) ;
#16165 = EDGE_CURVE ( 'NONE', #6925, #8823, #6161, .T. ) ;
#16166 = ORIENTED_EDGE ( 'NONE', *, *, #16650, .T. ) ;
#16167 = CARTESIAN_POINT ( 'NONE',  ( 9.346906861638174746, 42.80699732323137852, 76.23134092453109645 ) ) ;
#16168 =( NAMED_UNIT ( * ) PLANE_ANGLE_UNIT ( ) SI_UNIT ( $, .RADIAN. ) );
#16169 = CARTESIAN_POINT ( 'NONE',  ( 5.081851840395362530, 37.34681921564990859, 77.59303304176042104 ) ) ;
#16170 = EDGE_CURVE ( 'NONE', #16996, #5038, #1380, .T. ) ;
#16171 = CARTESIAN_POINT ( 'NONE',  ( 4.202107083175826929, 51.49017039810478735, 78.89819502495319625 ) ) ;
#16172 = CARTESIAN_POINT ( 'NONE',  ( 0.3279640439667344531, 52.35988168082469940, 78.50066232894263862 ) ) ;
#16173 = PLANE ( 'NONE',  #254 ) ;
#16174 = CARTESIAN_POINT ( 'NONE',  ( 0.3279640439667345642, 52.35988168082470651, 77.76169174070734869 ) ) ;
#16175 = CARTESIAN_POINT ( 'NONE',  ( 6.545534159973747990, 50.65336749702785113, 77.68963291717794561 ) ) ;
#16176 = CARTESIAN_POINT ( 'NONE',  ( 4.147036873812957047, 51.51748372786249064, 78.29064342123426457 ) ) ;
#16177 = CARTESIAN_POINT ( 'NONE',  ( -3.350035803220276609, 49.20851703305431357, 93.22683880123798872 ) ) ;
#16178 = ORIENTED_EDGE ( 'NONE', *, *, #191, .F. ) ;
#16179 = CARTESIAN_POINT ( 'NONE',  ( -5.086258153195711174, 37.36447471160525424, 79.53654225555244750 ) ) ;
#16180 = CARTESIAN_POINT ( 'NONE',  ( 8.951736416449948663, 41.62264642985666541, 78.48252796260671005 ) ) ;
#16181 = CARTESIAN_POINT ( 'NONE',  ( 5.298894634962917571, 50.82722828506639701, 78.90485198387828802 ) ) ;
#16182 = CARTESIAN_POINT ( 'NONE',  ( 8.375199775097003752, 41.81478521990748476, 77.14698585835439815 ) ) ;
#16183 = CARTESIAN_POINT ( 'NONE',  ( 8.621533274486752774, 40.63300666569625008, 75.47105533938442079 ) ) ;
#16184 = EDGE_LOOP ( 'NONE', ( #2725, #5923, #9051, #19289 ) ) ;
#16185 = CARTESIAN_POINT ( 'NONE',  ( 5.722750437672663892, 37.06256514788822898, 75.36130176902827316 ) ) ;
#16186 = CARTESIAN_POINT ( 'NONE',  ( 0.5975752275646775136, 52.20533044642586162, 79.54835876252475657 ) ) ;
#16187 = CARTESIAN_POINT ( 'NONE',  ( 6.395088259259853913, 38.46276872161406146, 77.80469260682309596 ) ) ;
#16188 = LINE ( 'NONE', #11725, #12814 ) ;
#16189 = LINE ( 'NONE', #11101, #19771 ) ;
#16190 = ORIENTED_EDGE ( 'NONE', *, *, #7622, .F. ) ;
#16191 = CARTESIAN_POINT ( 'NONE',  ( 26.43948732994507367, 45.16218137147968292, 74.70433879953098710 ) ) ;
#16192 = AXIS2_PLACEMENT_3D ( 'NONE', #8613, #5506, #18274 ) ;
#16193 = EDGE_LOOP ( 'NONE', ( #10039, #7404, #4816, #2256 ) ) ;
#16194 = CARTESIAN_POINT ( 'NONE',  ( 5.611423337425062385, 41.22389019960463230, 91.42996380123798872 ) ) ;
#16195 =( BOUNDED_CURVE ( )  B_SPLINE_CURVE ( 2, ( #11039, #19203, #15924, #6122, #2933, #1450, #3249, #2834, #14630, #6538, #14420 ),
 .UNSPECIFIED., .F., .T. ) 
 B_SPLINE_CURVE_WITH_KNOTS ( ( 3, 2, 2, 2, 2, 3 ),
 ( 0.3997652871908818351, 0.4062500000000000000, 0.4375000000000000000, 0.4687500000000000000, 0.5000000000000000000, 0.5173390146554853741 ),
 .UNSPECIFIED. ) 
 CURVE ( )  GEOMETRIC_REPRESENTATION_ITEM ( )  RATIONAL_B_SPLINE_CURVE ( ( 0.9749639670273970715, 0.9842041801420761127, 1.000000000000000000, 0.9238795325112867385, 1.000000000000000000, 0.9238795325112867385, 1.000000000000000000, 0.9238795325112867385, 1.000000000000000000, 0.9577646751561856853, 0.9623977609649205789 ) ) 
 REPRESENTATION_ITEM ( '' )  );
#16196 = CARTESIAN_POINT ( 'NONE',  ( -7.759339030830453510, 47.14028884343398573, 79.12207947904607863 ) ) ;
#16197 = CARTESIAN_POINT ( 'NONE',  ( -3.101538578788242351, 36.81245731659976883, 78.30834307773316993 ) ) ;
#16198 = CARTESIAN_POINT ( 'NONE',  ( -3.566438244846302119, 38.23101125920473464, 78.34992703482498655 ) ) ;
#16199 = LINE ( 'NONE', #5114, #15351 ) ;
#16200 = ORIENTED_EDGE ( 'NONE', *, *, #5248, .T. ) ;
#16201 = CARTESIAN_POINT ( 'NONE',  ( 8.722153740306486824, 36.96218137147968719, 95.05433879953098142 ) ) ;
#16202 = EDGE_LOOP ( 'NONE', ( #5927, #20794, #15828, #8284 ) ) ;
#16203 = AXIS2_PLACEMENT_3D ( 'NONE', #7445, #8843, #5308 ) ;
#16204 = B_SPLINE_CURVE_WITH_KNOTS ( 'NONE', 3,
 ( #4423, #15925, #12422, #17410, #10840, #17305, #1344, #8040, #1555, #2835, #20890, #6019, #3040, #14422, #12519, #20493, #4620, #5925 ),
 .UNSPECIFIED., .F., .F.,
 ( 4, 2, 2, 2, 2, 2, 2, 2, 4 ),
 ( 0.000000000000000000, 0.0003585842996636947450, 0.0007171685993273894900, 0.001075752898991083964, 0.001434337198654778546, 0.001792921498318473129, 0.001972213648150300362, 0.002151505797982128029, 0.002868674397309438698 ),
 .UNSPECIFIED. ) ;
#16205 = CARTESIAN_POINT ( 'NONE',  ( -2.914604833731050615, 51.60239615748798059, 76.69845644658968808 ) ) ;
#16206 = CARTESIAN_POINT ( 'NONE',  ( -2.416137431568557314, 39.07291177436112406, 91.27371380123798872 ) ) ;
#16207 = CARTESIAN_POINT ( 'NONE',  ( -4.567115856812060670, 47.10047254335474065, 94.55496380123798872 ) ) ;
#16208 = ORIENTED_EDGE ( 'NONE', *, *, #120, .F. ) ;
#16209 = CARTESIAN_POINT ( 'NONE',  ( -5.835675398032521777, 50.43488166173578691, 78.31711373209397209 ) ) ;
#16210 = CARTESIAN_POINT ( 'NONE',  ( -5.954796862783079625, 38.00602926950412552, 78.58503192925951453 ) ) ;
#16211 = CARTESIAN_POINT ( 'NONE',  ( -5.838428831739583380, 50.43291415881836315, 78.10580938776615767 ) ) ;
#16212 = CARTESIAN_POINT ( 'NONE',  ( 10.77494014480653561, 42.96218137147968008, 69.80574467885101342 ) ) ;
#16213 = EDGE_CURVE ( 'NONE', #4231, #2266, #11614, .T. ) ;
#16214 = CARTESIAN_POINT ( 'NONE',  ( 5.088724926954141026, 37.35642916330452579, 77.64535406911728899 ) ) ;
#16215 = ORIENTED_EDGE ( 'NONE', *, *, #12500, .T. ) ;
#16216 = CARTESIAN_POINT ( 'NONE',  ( -4.477846259693498254, 50.66218137147966871, 54.55433879953098852 ) ) ;
#16217 = LINE ( 'NONE', #9637, #2147 ) ;
#16218 = ORIENTED_EDGE ( 'NONE', *, *, #16339, .F. ) ;
#16219 = CARTESIAN_POINT ( 'NONE',  ( 4.987972048783305468, 51.80387588613526617, 77.70137231118654597 ) ) ;
#16220 = DIRECTION ( 'NONE',  ( 1.540237394707283727E-16, 1.793354297423763257E-16, -1.000000000000000000 ) ) ;
#16221 = CARTESIAN_POINT ( 'NONE',  ( -5.387797286270752828, 50.75491896253648605, 75.54244301425877950 ) ) ;
#16222 = CARTESIAN_POINT ( 'NONE',  ( -4.884656273474452526, 44.39824779480852612, 95.53246379611698558 ) ) ;
#16223 = VECTOR ( 'NONE', #1788, 1000.000000000000114 ) ;
#16224 = CARTESIAN_POINT ( 'NONE',  ( 0.7901638384306278740, 50.30062182352762079, 93.42308879782399345 ) ) ;
#16225 = LINE ( 'NONE', #4825, #7488 ) ;
#16226 = CARTESIAN_POINT ( 'NONE',  ( 5.611423337425062385, 41.22389019960463230, 90.17996380123798872 ) ) ;
#16227 = CARTESIAN_POINT ( 'NONE',  ( 5.579143690744149175, 50.61256526606223360, 76.32243632687685420 ) ) ;
#16228 = ADVANCED_FACE ( 'NONE', ( #4975 ), #17861, .T. ) ;
#16229 = ORIENTED_EDGE ( 'NONE', *, *, #12998, .T. ) ;
#16230 = CARTESIAN_POINT ( 'NONE',  ( 1.762171107682031002, 52.95697575291716674, 79.26556901187228732 ) ) ;
#16231 = VECTOR ( 'NONE', #17116, 1000.000000000000000 ) ;
#16232 = ORIENTED_EDGE ( 'NONE', *, *, #1302, .T. ) ;
#16233 = LINE ( 'NONE', #12726, #1367 ) ;
#16234 = LINE ( 'NONE', #17926, #8560 ) ;
#16235 = CARTESIAN_POINT ( 'NONE',  ( 9.307108147255313213, 42.68771805144258735, 79.03485483908291087 ) ) ;
#16236 = EDGE_CURVE ( 'NONE', #19441, #500, #12836, .T. ) ;
#16237 = CARTESIAN_POINT ( 'NONE',  ( -8.294722968033532595, 42.83806395776854714, 76.13058770837619704 ) ) ;
#16238 = EDGE_LOOP ( 'NONE', ( #15719, #6588, #11325, #14913, #12427, #13716, #8688, #4176, #17230, #16134, #8300, #9370, #8663 ) ) ;
#16239 = CARTESIAN_POINT ( 'NONE',  ( -5.154188915835984375, 42.64120994080404614, 93.61746380123797451 ) ) ;
#16240 = CARTESIAN_POINT ( 'NONE',  ( -5.046391490720765205, 38.27103331005528730, 75.52011153330033721 ) ) ;
#16241 = VERTEX_POINT ( 'NONE', #2007 ) ;
#16242 = VECTOR ( 'NONE', #18046, 1000.000000000000114 ) ;
#16243 = CARTESIAN_POINT ( 'NONE',  ( 2.122153740306508496, 49.76218137147969856, 77.55433879953099563 ) ) ;
#16244 = B_SPLINE_CURVE_WITH_KNOTS ( 'NONE', 3,
 ( #4953, #10187, #11881, #8478, #16670, #14855, #11472, #274, #14960, #9876, #175, #17944, #18156, #5262, #11778, #18254 ),
 .UNSPECIFIED., .F., .F.,
 ( 4, 2, 2, 2, 2, 2, 2, 4 ),
 ( 0.000000000000000000, 0.0002718550652617190348, 0.0005437101305234380696, 0.0008155651957851571586, 0.001087420261046876139, 0.001631130391570334483, 0.001902985456832064414, 0.002174840522093794346 ),
 .UNSPECIFIED. ) ;
#16245 = CARTESIAN_POINT ( 'NONE',  ( 8.378595026212774854, 41.81348187568733721, 78.70760583312296887 ) ) ;
#16246 = CARTESIAN_POINT ( 'NONE',  ( -2.904223097202481174, 48.62752260303690122, 96.27371379953099506 ) ) ;
#16247 = ORIENTED_EDGE ( 'NONE', *, *, #19610, .F. ) ;
#16248 = DIRECTION ( 'NONE',  ( 0.8136266022444372803, 0.5813877811927012917, 2.295812393977109100E-16 ) ) ;
#16249 = CARTESIAN_POINT ( 'NONE',  ( -6.739013063861042596, 40.35217951880748188, 78.85334789288012303 ) ) ;
#16250 = VERTEX_POINT ( 'NONE', #16273 ) ;
#16251 = CARTESIAN_POINT ( 'NONE',  ( -4.612897897929109980, 51.30863369456805145, 75.97269380145769446 ) ) ;
#16252 =( LENGTH_UNIT ( ) NAMED_UNIT ( * ) SI_UNIT ( .MILLI., .METRE. ) );
#16253 = FACE_OUTER_BOUND ( 'NONE', #9688, .T. ) ;
#16254 = EDGE_CURVE ( 'NONE', #4917, #19886, #13293, .T. ) ;
#16255 = VECTOR ( 'NONE', #11105, 1000.000000000000114 ) ;
#16256 = CARTESIAN_POINT ( 'NONE',  ( 5.939984016379080245, 38.00650938446680271, 78.33981856787941922 ) ) ;
#16257 = CARTESIAN_POINT ( 'NONE',  ( 8.869748494521283888, 41.37692342661967615, 77.52492703482499792 ) ) ;
#16258 = CARTESIAN_POINT ( 'NONE',  ( 0.09439724277526655161, 40.36218137147969998, 46.15433879953098284 ) ) ;
#16259 = EDGE_LOOP ( 'NONE', ( #19282, #7829 ) ) ;
#16260 = PLANE ( 'NONE',  #3716 ) ;
#16261 = CARTESIAN_POINT ( 'NONE',  ( 9.353743827924017040, 42.82748814491910139, 76.70850639745313515 ) ) ;
#16262 = CARTESIAN_POINT ( 'NONE',  ( 27.27315414062681853, 40.36218137147969287, 105.5543387995309956 ) ) ;
#16263 = CARTESIAN_POINT ( 'NONE',  ( 6.436934174446692580, 49.81957092643428808, 78.08828162113617566 ) ) ;
#16264 = AXIS2_PLACEMENT_3D ( 'NONE', #17168, #18766, #2590 ) ;
#16265 = ORIENTED_EDGE ( 'NONE', *, *, #1977, .F. ) ;
#16266 = ORIENTED_EDGE ( 'NONE', *, *, #8821, .T. ) ;
#16267 = EDGE_CURVE ( 'NONE', #13330, #20802, #19765, .T. ) ;
#16268 = CARTESIAN_POINT ( 'NONE',  ( 7.739670491838285038, 40.27007090160952174, 75.95778646784575017 ) ) ;
#16270 = EDGE_CURVE ( 'NONE', #9248, #15579, #15015, .T. ) ;
#16269 = CARTESIAN_POINT ( 'NONE',  ( 2.522153740306509295, 50.16218137147969713, 61.55433879953100273 ) ) ;
#16271 = CARTESIAN_POINT ( 'NONE',  ( 0.5221537403065008576, 44.16218137147969003, 105.5543387995310098 ) ) ;
#16272 = CARTESIAN_POINT ( 'NONE',  ( 5.939900590116411472, 51.10072461867315496, 76.90580938776616904 ) ) ;
#16273 = CARTESIAN_POINT ( 'NONE',  ( -7.079975527142585712, 43.92211762787398044, 75.45433879953087342 ) ) ;
#16274 = FACE_OUTER_BOUND ( 'NONE', #10241, .T. ) ;
#16275 = CARTESIAN_POINT ( 'NONE',  ( 0.5221537403065188432, 44.16218137147969003, 54.55433879953099563 ) ) ;
#16276 = CARTESIAN_POINT ( 'NONE',  ( 4.293446294024885646, 51.44367749308788973, 77.90149807450526964 ) ) ;
#16277 = FACE_OUTER_BOUND ( 'NONE', #19417, .T. ) ;
#16278 = ADVANCED_FACE ( 'NONE', ( #16382 ), #8293, .F. ) ;
#16279 = VECTOR ( 'NONE', #8096, 1000.000000000000000 ) ;
#16280 = ADVANCED_FACE ( 'NONE', ( #10215 ), #16693, .F. ) ;
#16281 = CARTESIAN_POINT ( 'NONE',  ( 4.394343283833276992, 39.11584570990505938, 93.85183880123797451 ) ) ;
#16282 = ORIENTED_EDGE ( 'NONE', *, *, #11974, .T. ) ;
#16283 = CARTESIAN_POINT ( 'NONE',  ( 8.837344731589769964, 41.27980729345753730, 78.92656146296575059 ) ) ;
#16284 = CARTESIAN_POINT ( 'NONE',  ( 8.941920682866751235, 41.59322805360929465, 78.83412695248559032 ) ) ;
#16285 = LINE ( 'NONE', #14473, #17430 ) ;
#16286 = DIRECTION ( 'NONE',  ( 0.007885122365275663500, 0.9999689119394085113, 1.805443505845543142E-16 ) ) ;
#16287 = CARTESIAN_POINT ( 'NONE',  ( 8.387016861607721196, 39.93014609885396027, 76.70090004521539129 ) ) ;
#16288 = VERTEX_POINT ( 'NONE', #934 ) ;
#16289 = ORIENTED_EDGE ( 'NONE', *, *, #2896, .F. ) ;
#16290 = VECTOR ( 'NONE', #12009, 1000.000000000000000 ) ;
#16291 = FACE_OUTER_BOUND ( 'NONE', #18394, .T. ) ;
#16292 = LINE ( 'NONE', #3205, #17632 ) ;
#16293 = CARTESIAN_POINT ( 'NONE',  ( 6.447652509444688818, 38.50032921029611543, 77.26022115247205591 ) ) ;
#16294 = CARTESIAN_POINT ( 'NONE',  ( -3.501354354950023229, 36.19377011966047775, 76.40804902690982203 ) ) ;
#16295 = FACE_OUTER_BOUND ( 'NONE', #17286, .T. ) ;
#16296 = ORIENTED_EDGE ( 'NONE', *, *, #120, .T. ) ;
#16297 = CARTESIAN_POINT ( 'NONE',  ( 8.947997572694543322, 41.61144087793389446, 76.20405737193274831 ) ) ;
#16298 = AXIS2_PLACEMENT_3D ( 'NONE', #11452, #9963, #6534 ) ;
#16299 = ORIENTED_EDGE ( 'NONE', *, *, #5211, .T. ) ;
#16300 = CARTESIAN_POINT ( 'NONE',  ( -4.567115856812060670, 47.10047254335474065, 90.80496380123797451 ) ) ;
#16301 = ADVANCED_FACE ( 'NONE', ( #18598 ), #17216, .F. ) ;
#16302 = VECTOR ( 'NONE', #20475, 1000.000000000000000 ) ;
#16303 = CARTESIAN_POINT ( 'NONE',  ( 1.251324093324716946, 52.20841207932105021, 76.78082255713043480 ) ) ;
#16304 = DIRECTION ( 'NONE',  ( -1.110223024625156540E-16, -1.000000000000000000, -5.922860397471808077E-17 ) ) ;
#16305 = CARTESIAN_POINT ( 'NONE',  ( 8.314165830633189813, 41.60776736370225848, 75.97520393624411383 ) ) ;
#16306 = VECTOR ( 'NONE', #12434, 1000.000000000000114 ) ;
#16307 = AXIS2_PLACEMENT_3D ( 'NONE', #3583, #18264, #13383 ) ;
#16308 = CARTESIAN_POINT ( 'NONE',  ( 8.639127872212812420, 42.99760432031693824, 78.86684150954961581 ) ) ;
#16309 = EDGE_LOOP ( 'NONE', ( #16833, #6689, #19984, #16265 ) ) ;
#16310 = ORIENTED_EDGE ( 'NONE', *, *, #12879, .T. ) ;
#16311 = VECTOR ( 'NONE', #7950, 1000.000000000000000 ) ;
#16312 = CARTESIAN_POINT ( 'NONE',  ( -2.503296703960768088, 48.49064145155251992, 92.86279910766216972 ) ) ;
#16313 = VECTOR ( 'NONE', #12119, 1000.000000000000000 ) ;
#16314 = CARTESIAN_POINT ( 'NONE',  ( 6.198496396448986090, 45.68315280215533392, 91.74246380123798872 ) ) ;
#16315 = CARTESIAN_POINT ( 'NONE',  ( -0.4699484075730043786, 51.36218137147968577, 48.36106904222365444 ) ) ;
#16316 = VERTEX_POINT ( 'NONE', #15309 ) ;
#16317 = CARTESIAN_POINT ( 'NONE',  ( 0.5706356501935867520, 52.36203804732553380, 75.97198585835440099 ) ) ;
#16318 = CARTESIAN_POINT ( 'NONE',  ( 0.5221537403065020788, 52.36218137147968577, 87.21440135111343750 ) ) ;
#16319 = CARTESIAN_POINT ( 'NONE',  ( 5.740585635973905809, 51.24795054640212300, 75.97198585835440099 ) ) ;
#16320 = DIRECTION ( 'NONE',  ( 1.540237394707284220E-16, 1.793354297423764243E-16, -1.000000000000000000 ) ) ;
#16321 = CARTESIAN_POINT ( 'NONE',  ( 23.03948732994508575, 45.16218137147969003, 76.90433879953100416 ) ) ;
#16322 = ORIENTED_EDGE ( 'NONE', *, *, #20561, .F. ) ;
#16323 = AXIS2_PLACEMENT_3D ( 'NONE', #17092, #15282, #18790 ) ;
#16324 = CARTESIAN_POINT ( 'NONE',  ( -4.095068233311042860, 50.93174038172981000, 76.01002907825849775 ) ) ;
#16325 = VECTOR ( 'NONE', #11529, 1000.000000000000000 ) ;
#16326 = DIRECTION ( 'NONE',  ( -0.009567942452870459302, 0.9999542261909885044, 1.778535306010345054E-16 ) ) ;
#16327 = VERTEX_POINT ( 'NONE', #2640 ) ;
#16328 = CARTESIAN_POINT ( 'NONE',  ( 2.548566262980702213, 48.91524988949119290, 95.05433879953096721 ) ) ;
#16329 = CARTESIAN_POINT ( 'NONE',  ( -6.794221408397769224, 40.57951578525081260, 77.67144260532384692 ) ) ;
#16330 = CARTESIAN_POINT ( 'NONE',  ( 0.5221537403065010796, 44.16218137147969003, 77.84651775085080772 ) ) ;
#16331 = CARTESIAN_POINT ( 'NONE',  ( -1.590937568396971091, 39.63064243629642647, 95.76683879611698558 ) ) ;
#16332 = VECTOR ( 'NONE', #9553, 1000.000000000000227 ) ;
#16333 = CARTESIAN_POINT ( 'NONE',  ( 0.2541436421823711211, 38.02374091943176637, 92.79808879782397923 ) ) ;
#16334 = CARTESIAN_POINT ( 'NONE',  ( -3.137939750588703003, 36.85016333763859109, 77.38751485876633751 ) ) ;
#16335 = ORIENTED_EDGE ( 'NONE', *, *, #9049, .F. ) ;
#16336 = DIRECTION ( 'NONE',  ( 2.409338161078896715E-16, -1.000000000000000000, 0.000000000000000000 ) ) ;
#16337 = AXIS2_PLACEMENT_3D ( 'NONE', #177, #6661, #6964 ) ;
#16338 = CARTESIAN_POINT ( 'NONE',  ( -5.531051774427891310, 44.10426199826898142, 75.45433879953087342 ) ) ;
#16339 = EDGE_CURVE ( 'NONE', #4614, #16577, #4225, .T. ) ;
#16340 = ORIENTED_EDGE ( 'NONE', *, *, #8421, .F. ) ;
#16341 = CARTESIAN_POINT ( 'NONE',  ( 1.250118884985844225, 46.34393909133126499, 82.45433879953087342 ) ) ;
#16342 = CARTESIAN_POINT ( 'NONE',  ( 30.92220646078100188, 42.76218137147968434, 62.80715055817104542 ) ) ;
#16343 = LINE ( 'NONE', #7836, #13661 ) ;
#16344 = VERTEX_POINT ( 'NONE', #3907 ) ;
#16345 = LINE ( 'NONE', #20803, #14281 ) ;
#16346 = CARTESIAN_POINT ( 'NONE',  ( -5.950833756536988872, 38.00310188256379007, 76.46818962967083166 ) ) ;
#16347 = EDGE_LOOP ( 'NONE', ( #18515, #8787, #18886, #1591 ) ) ;
#16348 = DIRECTION ( 'NONE',  ( -0.5941461771851693774, -0.8043570849667760481, -2.357623395011396791E-16 ) ) ;
#16349 = CARTESIAN_POINT ( 'NONE',  ( 32.52215374030649286, 44.16218137147969003, 87.85433879953103542 ) ) ;
#16350 = DIRECTION ( 'NONE',  ( -0.8136266022444372803, -0.5813877811927012917, -2.295812393977109100E-16 ) ) ;
#16351 = ORIENTED_EDGE ( 'NONE', *, *, #19611, .F. ) ;
#16352 = CARTESIAN_POINT ( 'NONE',  ( 0.5221537403065094063, 50.16218137147969713, 61.15433879953099705 ) ) ;
#16353 = CARTESIAN_POINT ( 'NONE',  ( 25.03948732994508219, 36.35905713404684292, 74.70433879953100131 ) ) ;
#16354 = CARTESIAN_POINT ( 'NONE',  ( -4.009385194876761815, 46.27527268018315709, 93.26683879953097289 ) ) ;
#16355 = EDGE_CURVE ( 'NONE', #12967, #7893, #12220, .T. ) ;
#16356 = ORIENTED_EDGE ( 'NONE', *, *, #15993, .F. ) ;
#16357 = CARTESIAN_POINT ( 'NONE',  ( -7.866550369700228806, 41.50330127738815378, 78.93669174070734584 ) ) ;
#16358 = CARTESIAN_POINT ( 'NONE',  ( 8.889576793745449734, 46.88836537034026719, 78.73595644658969661 ) ) ;
#16359 = DIRECTION ( 'NONE',  ( 0.5735764363510442720, -0.8191520442889930198, -0.000000000000000000 ) ) ;
#16360 = CARTESIAN_POINT ( 'NONE',  ( -5.784195910403845176, 44.99242805365518194, 94.63308880123798872 ) ) ;
#16361 = CARTESIAN_POINT ( 'NONE',  ( 6.025664479182668565, 50.11254134161350038, 75.49932683761802821 ) ) ;
#16362 = CARTESIAN_POINT ( 'NONE',  ( 8.214799251806553571, 41.32260305165857517, 72.45433879953087342 ) ) ;
#16363 = CARTESIAN_POINT ( 'NONE',  ( 0.5221537403065086291, 44.16218137147969713, 61.55433879953100273 ) ) ;
#16364 = CARTESIAN_POINT ( 'NONE',  ( 4.681897302132870919, 37.23858518757540281, 75.43572969368668168 ) ) ;
#16365 = DIRECTION ( 'NONE',  ( -1.000000000000000000, 1.110223024625156540E-16, -1.779391786395883043E-16 ) ) ;
#16366 = EDGE_CURVE ( 'NONE', #14291, #18616, #10533, .T. ) ;
#16367 = ORIENTED_EDGE ( 'NONE', *, *, #15463, .T. ) ;
#16368 = VECTOR ( 'NONE', #15134, 1000.000000000000000 ) ;
#16369 = CARTESIAN_POINT ( 'NONE',  ( -4.361665858399769391, 37.57520132541210245, 75.97198585835440099 ) ) ;
#16370 = CARTESIAN_POINT ( 'NONE',  ( 9.271487163511554996, 42.58095970340946934, 75.72637824826109920 ) ) ;
#16371 = CARTESIAN_POINT ( 'NONE',  ( -7.376743071288318632, 41.96049357349896525, 78.13669174070733447 ) ) ;
#16372 = CARTESIAN_POINT ( 'NONE',  ( 6.575642869179847416, 50.63112740639009246, 77.70577767651062118 ) ) ;
#16373 = VECTOR ( 'NONE', #11923, 1000.000000000000227 ) ;
#16374 = ORIENTED_EDGE ( 'NONE', *, *, #10808, .F. ) ;
#16375 = CARTESIAN_POINT ( 'NONE',  ( 5.853612939038055352, 51.16446183064613251, 78.89719962956496602 ) ) ;
#16376 = B_SPLINE_CURVE_WITH_KNOTS ( 'NONE', 3,
 ( #1323, #7808, #14293, #18882, #20769, #1531 ),
 .UNSPECIFIED., .F., .F.,
 ( 4, 2, 4 ),
 ( 0.000000000000000000, 0.002233029297497547087, 0.004466058594995094173 ),
 .UNSPECIFIED. ) ;
#16377 = VERTEX_POINT ( 'NONE', #16798 ) ;
#16378 = EDGE_CURVE ( 'NONE', #15919, #1549, #2216, .T. ) ;
#16379 = CARTESIAN_POINT ( 'NONE',  ( 4.973101328672442811, 51.81486028805201727, 77.67439681936272677 ) ) ;
#16380 = DIRECTION ( 'NONE',  ( -0.9534635866061492715, -0.3015081906286096181, -2.009271279954799034E-16 ) ) ;
#16381 = FACE_OUTER_BOUND ( 'NONE', #2937, .T. ) ;
#16382 = FACE_OUTER_BOUND ( 'NONE', #2236, .T. ) ;
#16383 = CYLINDRICAL_SURFACE ( 'NONE', #20632, 3.999999999999996447 ) ;
#16384 = EDGE_CURVE ( 'NONE', #13636, #16959, #12333, .T. ) ;
#16385 = VECTOR ( 'NONE', #4795, 1000.000000000000227 ) ;
#16386 = CARTESIAN_POINT ( 'NONE',  ( 11.22215374030649926, 42.96218137147968008, 77.80433879953099563 ) ) ;
#16387 = FACE_OUTER_BOUND ( 'NONE', #17941, .T. ) ;
#16388 = CARTESIAN_POINT ( 'NONE',  ( -4.526965251788245936, 37.70598351703077356, 76.16751655709613544 ) ) ;
#16389 = VECTOR ( 'NONE', #12011, 1000.000000000000000 ) ;
#16390 = CARTESIAN_POINT ( 'NONE',  ( 5.568489401881125289, 48.03437091500646261, 91.66433880123796030 ) ) ;
#16391 = ORIENTED_EDGE ( 'NONE', *, *, #19583, .T. ) ;
#16392 = CARTESIAN_POINT ( 'NONE',  ( 8.865792162213244509, 41.36506604770743678, 78.93669174070734584 ) ) ;
#16393 = ADVANCED_FACE ( 'NONE', ( #8713 ), #17115, .F. ) ;
#16394 = ADVANCED_FACE ( 'NONE', ( #12116 ), #17192, .T. ) ;
#16395 = CARTESIAN_POINT ( 'NONE',  ( 8.950958007118590132, 41.62031348770922534, 78.64183653779139149 ) ) ;
#16396 = ADVANCED_FACE ( 'NONE', ( #15498 ), #12094, .F. ) ;
#16397 = CARTESIAN_POINT ( 'NONE',  ( 8.648170029844118645, 43.06315486489794608, 76.74257409364851412 ) ) ;
#16398 = CARTESIAN_POINT ( 'NONE',  ( 8.876519138579782364, 41.39721547638464472, 77.52397343602532942 ) ) ;
#16399 = EDGE_CURVE ( 'NONE', #18638, #14895, #5688, .T. ) ;
#16400 = VECTOR ( 'NONE', #4036, 1000.000000000000000 ) ;
#16401 = CARTESIAN_POINT ( 'NONE',  ( 8.475713225669114337, 40.19597472873837063, 75.74322883085581282 ) ) ;
#16402 = ORIENTED_EDGE ( 'NONE', *, *, #11741, .T. ) ;
#16403 = ORIENTED_EDGE ( 'NONE', *, *, #20820, .F. ) ;
#16404 = CARTESIAN_POINT ( 'NONE',  ( 6.416235914874578228, 38.47788006205125555, 76.12774863075016185 ) ) ;
#16405 = CARTESIAN_POINT ( 'NONE',  ( -0.02252005271732430980, 52.21022012559965475, 79.48573486738433758 ) ) ;
#16406 = CARTESIAN_POINT ( 'NONE',  ( -5.412716252285423302, 48.91899944357702879, 75.45433879953087342 ) ) ;
#16407 = CARTESIAN_POINT ( 'NONE',  ( 4.324106654390397431, 51.42778090780855393, 75.70619357739094824 ) ) ;
#16408 = CARTESIAN_POINT ( 'NONE',  ( 5.391786323697940198, 50.75965653268888644, 77.94845644658968808 ) ) ;
#16409 = EDGE_LOOP ( 'NONE', ( #1143, #7708, #17198 ) ) ;
#16410 = ADVANCED_FACE ( 'NONE', ( #4095 ), #19351, .F. ) ;
#16411 = LINE ( 'NONE', #6597, #10118 ) ;
#16412 = VERTEX_POINT ( 'NONE', #14828 ) ;
#16413 = CARTESIAN_POINT ( 'NONE',  ( -0.9988176903691428077, 49.83852402762217082, 90.64871380123798872 ) ) ;
#16414 = CARTESIAN_POINT ( 'NONE',  ( 2.021804202196959555, 52.20233656050648818, 77.22796645847455466 ) ) ;
#16415 = B_SPLINE_CURVE_WITH_KNOTS ( 'NONE', 3,
 ( #14459, #5082, #16480, #14872, #292, #20924, #12860, #16167, #6785, #13289, #9579, #11175, #16065, #8072, #14565, #609, #5183, #12019, #5283, #13704, #19862, #16584, #10212 ),
 .UNSPECIFIED., .F., .F.,
 ( 4, 1, 1, 1, 1, 1, 1, 1, 1, 1, 1, 1, 1, 1, 1, 1, 1, 1, 1, 1, 4 ),
 ( 0.000000000000000000, 0.04300144207505136179, 0.08353165498080591944, 0.1209955408344369626, 0.1553840623654753617, 0.1873435814759382700, 0.2162479910858959298, 0.2424976236983500399, 0.2660452007499324312, 0.3104933729322157387, 0.3556083049253406791, 0.4034864083407884716, 0.4540969056831142825, 0.5078508224766279389, 0.5647468969590679899, 0.6259022191770886590, 0.6917657563094725681, 0.7621492621511971599, 0.8365553829333508551, 0.9158190838930461153, 1.000000000000000000 ),
 .UNSPECIFIED. ) ;
#16416 = FACE_OUTER_BOUND ( 'NONE', #818, .T. ) ;
#16417 = CIRCLE ( 'NONE', #18392, 6.200000000000000178 ) ;
#16418 = DIRECTION ( 'NONE',  ( -0.9480563259966798828, -0.3181025035074024343, -2.030702297275143506E-16 ) ) ;
#16419 = ORIENTED_EDGE ( 'NONE', *, *, #20414, .F. ) ;
#16420 = EDGE_CURVE ( 'NONE', #3871, #3020, #7238, .T. ) ;
#16421 = LINE ( 'NONE', #11738, #12486 ) ;
#16422 = ORIENTED_EDGE ( 'NONE', *, *, #9620, .T. ) ;
#16423 = CARTESIAN_POINT ( 'NONE',  ( 1.652727357819364418, 35.35299279957455099, 76.86610350541323555 ) ) ;
#16424 = EDGE_CURVE ( 'NONE', #19082, #10941, #9482, .T. ) ;
#16425 = CARTESIAN_POINT ( 'NONE',  ( 2.043125170982144745, 38.48583871533720213, 91.42996380123798872 ) ) ;
#16426 = FACE_OUTER_BOUND ( 'NONE', #19730, .T. ) ;
#16427 = EDGE_LOOP ( 'NONE', ( #17132, #13466, #11090, #13566 ) ) ;
#16428 = CARTESIAN_POINT ( 'NONE',  ( 0.5221537403065015237, 49.16218137147969003, 92.72886871425484401 ) ) ;
#16429 = FACE_OUTER_BOUND ( 'NONE', #12985, .T. ) ;
#16430 = CIRCLE ( 'NONE', #19808, 8.199999999999999289 ) ;
#16431 = DIRECTION ( 'NONE',  ( 1.239088197126290817E-16, 1.000000000000000000, 0.000000000000000000 ) ) ;
#16432 = LINE ( 'NONE', #6725, #2012 ) ;
#16433 = CARTESIAN_POINT ( 'NONE',  ( 3.547567743947607877, 48.49067789217865254, 93.48725702289965511 ) ) ;
#16434 = EDGE_LOOP ( 'NONE', ( #8751, #11837, #19905, #20987 ) ) ;
#16435 = CARTESIAN_POINT ( 'NONE',  ( -1.477846259693492481, 49.76218137147968434, 69.55433879953100984 ) ) ;
#16436 = CARTESIAN_POINT ( 'NONE',  ( 0.8402443429964431276, 52.35221751176949567, 78.65078808693101564 ) ) ;
#16437 = ORIENTED_EDGE ( 'NONE', *, *, #14698, .T. ) ;
#16438 = CARTESIAN_POINT ( 'NONE',  ( 4.572162582958037014, 51.19700258348528621, 77.68963291717793140 ) ) ;
#16439 = FACE_OUTER_BOUND ( 'NONE', #18648, .T. ) ;
#16440 = DIRECTION ( 'NONE',  ( 1.193617070626243484E-16, 1.000000000000000000, 0.000000000000000000 ) ) ;
#16441 = CARTESIAN_POINT ( 'NONE',  ( -4.176309363623030180, 42.45208065485131499, 93.11058879611698558 ) ) ;
#16442 = DIRECTION ( 'NONE',  ( 1.779391786395883536E-16, 5.922860397471806844E-17, -1.000000000000000000 ) ) ;
#16443 = CARTESIAN_POINT ( 'NONE',  ( 9.353817388681445522, 42.82770861117572281, 76.74257409364852833 ) ) ;
#16444 = DIRECTION ( 'NONE',  ( -0.000000000000000000, 1.000000000000000000, -0.000000000000000000 ) ) ;
#16445 = AXIS2_PLACEMENT_3D ( 'NONE', #1648, #8243, #6416 ) ;
#16446 = EDGE_LOOP ( 'NONE', ( #1506, #1189, #7363, #20295, #6847, #4474, #5576, #3655, #2452, #3587, #5352, #14427, #14751, #14979, #5193, #13256, #9917, #20123, #18465, #19830, #9066, #2487, #9190, #4726, #20244, #10669, #11005, #14287, #14494, #11566, #9098, #3795, #8528, #11731, #3877, #526, #6806, #15393, #19682, #3689 ) ) ;
#16447 = CARTESIAN_POINT ( 'NONE',  ( 8.951667845840693971, 41.62244091939069790, 76.38301527011910252 ) ) ;
#16448 = CARTESIAN_POINT ( 'NONE',  ( 5.389492195292208798, 36.82443100924615464, 78.09625056423674039 ) ) ;
#16449 = ORIENTED_EDGE ( 'NONE', *, *, #11071, .F. ) ;
#16450 = FACE_BOUND ( 'NONE', #4383, .T. ) ;
#16451 = CARTESIAN_POINT ( 'NONE',  ( -5.529385682154831727, 44.31555110708731604, 75.45433879953087342 ) ) ;
#16452 = CARTESIAN_POINT ( 'NONE',  ( -5.058133621542618030, 44.89684013992257405, 96.42996379953098085 ) ) ;
#16453 = ORIENTED_EDGE ( 'NONE', *, *, #16914, .F. ) ;
#16454 = CARTESIAN_POINT ( 'NONE',  ( -5.474200200999507437, 38.58703837115216828, 76.14635491738357587 ) ) ;
#16455 = ORIENTED_EDGE ( 'NONE', *, *, #18724, .F. ) ;
#16456 = DIRECTION ( 'NONE',  ( -0.5813877811927011807, 0.8136266022444372803, 5.636455622144619183E-17 ) ) ;
#16457 = CARTESIAN_POINT ( 'NONE',  ( 0.3351286093508437092, 52.96019378912382791, 76.24030412541705459 ) ) ;
#16458 = CARTESIAN_POINT ( 'NONE',  ( -4.500660556396669065, 42.81632233694663370, 94.00808879953098085 ) ) ;
#16459 = ORIENTED_EDGE ( 'NONE', *, *, #9120, .T. ) ;
#16460 = CARTESIAN_POINT ( 'NONE',  ( -4.517072128342596748, 36.94403992325786135, 78.34992703482498655 ) ) ;
#16461 = ORIENTED_EDGE ( 'NONE', *, *, #6047, .F. ) ;
#16462 = CARTESIAN_POINT ( 'NONE',  ( 6.575359255040893913, 44.22010074469034180, 72.45433879953087342 ) ) ;
#16463 = CARTESIAN_POINT ( 'NONE',  ( 0.3279640439667344531, 52.35988168082469940, 78.50066232894263862 ) ) ;
#16464 = CARTESIAN_POINT ( 'NONE',  ( -5.154188915835984375, 42.64120994080404614, 94.71121380123797451 ) ) ;
#16465 =( NAMED_UNIT ( * ) SI_UNIT ( $, .STERADIAN. ) SOLID_ANGLE_UNIT ( ) );
#16466 = CARTESIAN_POINT ( 'NONE',  ( 5.417149068951104596, 50.56202716265563168, 75.36137945677606353 ) ) ;
#16467 = DIRECTION ( 'NONE',  ( -1.540237394707284220E-16, -1.793354297423764243E-16, 1.000000000000000000 ) ) ;
#16468 = B_SPLINE_CURVE_WITH_KNOTS ( 'NONE', 3,
 ( #6919, #320, #19791, #3935, #5213, #11730, #18303, #20102, #19892, #11828, #16613 ),
 .UNSPECIFIED., .F., .F.,
 ( 4, 1, 1, 1, 1, 1, 1, 1, 4 ),
 ( 0.000000000000000000, 0.2014779019512820402, 0.3683355476270177564, 0.4986267722911685296, 0.6014797591950403755, 0.6911751734036410966, 0.7846115128848750730, 0.8848135988872103397, 1.000000000000000000 ),
 .UNSPECIFIED. ) ;
#16469 = CARTESIAN_POINT ( 'NONE',  ( 4.464802119779007761, 36.16368133634887982, 76.05895398371444571 ) ) ;
#16470 = VERTEX_POINT ( 'NONE', #562 ) ;
#16471 = PLANE ( 'NONE',  #4724 ) ;
#16472 = CARTESIAN_POINT ( 'NONE',  ( 9.240682951717872129, 42.48863752648103542, 75.64289537645213102 ) ) ;
#16473 = CARTESIAN_POINT ( 'NONE',  ( 0.5221537403065097394, 44.16218137147969003, 111.0905869729573681 ) ) ;
#16474 = CARTESIAN_POINT ( 'NONE',  ( -7.723582874747324745, 47.23591325229828186, 75.45433879953087342 ) ) ;
#16475 = ORIENTED_EDGE ( 'NONE', *, *, #7153, .F. ) ;
#16476 = ORIENTED_EDGE ( 'NONE', *, *, #1692, .F. ) ;
#16477 = CARTESIAN_POINT ( 'NONE',  ( -4.895593109503407980, 37.22363812428621088, 78.18375056423674607 ) ) ;
#16478 = EDGE_LOOP ( 'NONE', ( #11247, #12466, #3659, #6022 ) ) ;
#16479 = CARTESIAN_POINT ( 'NONE',  ( -3.557428649121368469, 36.23518994195450205, 77.32142682847380399 ) ) ;
#16480 = CARTESIAN_POINT ( 'NONE',  ( 9.353600933836910158, 42.82705988227500882, 76.64232882509132594 ) ) ;
#16481 = DIRECTION ( 'NONE',  ( -0.8236492988270761595, -0.5670994908670485835, -2.285625759191147486E-16 ) ) ;
#16482 = CARTESIAN_POINT ( 'NONE',  ( -1.219503646467431590, 49.90383875825363447, 61.41268141275705972 ) ) ;
#16483 = EDGE_CURVE ( 'NONE', #10143, #13698, #9428, .T. ) ;
#16484 = CARTESIAN_POINT ( 'NONE',  ( 0.7901638384306279850, 50.30062182352762079, 93.42308879782399345 ) ) ;
#16485 = CARTESIAN_POINT ( 'NONE',  ( 5.599418364623888422, 51.35222512318382826, 78.27515171461519117 ) ) ;
#16486 = LINE ( 'NONE', #615, #10570 ) ;
#16487 = CARTESIAN_POINT ( 'NONE',  ( 4.198599642040965030, 51.49202303595968999, 78.03894196152546670 ) ) ;
#16488 = CARTESIAN_POINT ( 'NONE',  ( -0.9988176903691428077, 49.83852402762217082, 91.89871380123798872 ) ) ;
#16489 = CARTESIAN_POINT ( 'NONE',  ( 5.568489401881125289, 48.03437091500646261, 92.91433880123798872 ) ) ;
#16490 = ORIENTED_EDGE ( 'NONE', *, *, #3242, .T. ) ;
#16491 = CARTESIAN_POINT ( 'NONE',  ( 0.3327557958309655950, 52.96755809673673099, 76.44919174070734869 ) ) ;
#16492 = VERTEX_POINT ( 'NONE', #15046 ) ;
#16493 = EDGE_CURVE ( 'NONE', #10557, #7365, #5748, .T. ) ;
#16494 = CARTESIAN_POINT ( 'NONE',  ( 8.951433321995803993, 41.62173803654965099, 78.54183882225588320 ) ) ;
#16495 = CARTESIAN_POINT ( 'NONE',  ( -4.534948301111438873, 37.71188027398896736, 78.53742703482498655 ) ) ;
#16496 = LINE ( 'NONE', #1914, #1383 ) ;
#16497 = EDGE_CURVE ( 'NONE', #17442, #3406, #16952, .T. ) ;
#16498 = CARTESIAN_POINT ( 'NONE',  ( 8.648380609495486482, 40.71346983188059454, 75.44378286633819641 ) ) ;
#16499 = VERTEX_POINT ( 'NONE', #19918 ) ;
#16500 = ORIENTED_EDGE ( 'NONE', *, *, #7272, .T. ) ;
#16501 = CARTESIAN_POINT ( 'NONE',  ( -4.176309363623031068, 42.45208065485131499, 94.36058879611698558 ) ) ;
#16502 = CARTESIAN_POINT ( 'NONE',  ( 7.866866907225194439, 40.51444835331399474, 79.25767082237931049 ) ) ;
#16503 = CARTESIAN_POINT ( 'NONE',  ( -3.538420156175611009, 36.22114913392427127, 76.12177974158937843 ) ) ;
#16504 = CARTESIAN_POINT ( 'NONE',  ( 0.8450176760924454911, 52.95625770591603754, 76.16933217328414685 ) ) ;
#16505 = ORIENTED_EDGE ( 'NONE', *, *, #3385, .T. ) ;
#16506 =( BOUNDED_CURVE ( )  B_SPLINE_CURVE ( 3, ( #17681, #14276, #1518, #3110 ),
 .UNSPECIFIED., .F., .F. ) 
 B_SPLINE_CURVE_WITH_KNOTS ( ( 4, 4 ),
 ( 1.579404754493129337, 1.650417730407532479 ),
 .UNSPECIFIED. ) 
 CURVE ( )  GEOMETRIC_REPRESENTATION_ITEM ( )  RATIONAL_B_SPLINE_CURVE ( ( 1.000000000000000000, 0.9995798072522218414, 0.9995798072522218414, 1.000000000000000000 ) ) 
 REPRESENTATION_ITEM ( '' )  );
#16507 = EDGE_CURVE ( 'NONE', #1035, #13218, #13544, .T. ) ;
#16508 = CARTESIAN_POINT ( 'NONE',  ( 8.949991632966883159, 41.61741720307092152, 76.25788209700408515 ) ) ;
#16509 = EDGE_CURVE ( 'NONE', #14083, #6021, #17559, .T. ) ;
#16510 = DIRECTION ( 'NONE',  ( -0.003070188988870460947, 0.009708901767422541129, 0.9999481542390301625 ) ) ;
#16511 = ORIENTED_EDGE ( 'NONE', *, *, #3228, .T. ) ;
#16512 = CARTESIAN_POINT ( 'NONE',  ( 3.948530577815480225, 39.69684013992245752, 94.71121380294496817 ) ) ;
#16513 = CARTESIAN_POINT ( 'NONE',  ( -7.863115711494208071, 41.48039487425794647, 78.93576421268289778 ) ) ;
#16514 = EDGE_CURVE ( 'NONE', #9686, #17850, #15815, .T. ) ;
#16515 = CARTESIAN_POINT ( 'NONE',  ( 6.198496396448986090, 45.68315280215533392, 95.33621380123798872 ) ) ;
#16516 = LINE ( 'NONE', #5220, #1078 ) ;
#16517 = ORIENTED_EDGE ( 'NONE', *, *, #18715, .T. ) ;
#16518 = LINE ( 'NONE', #18212, #1123 ) ;
#16519 = ORIENTED_EDGE ( 'NONE', *, *, #913, .T. ) ;
#16520 = LINE ( 'NONE', #229, #11564 ) ;
#16521 = DIRECTION ( 'NONE',  ( -0.9999689119394086223, 0.007885122365275665235, -1.526048693634353392E-16 ) ) ;
#16522 = ORIENTED_EDGE ( 'NONE', *, *, #12127, .F. ) ;
#16523 = CARTESIAN_POINT ( 'NONE',  ( -1.202011496911927324, 49.96493122755408223, 72.45433879953087342 ) ) ;
#16524 = CARTESIAN_POINT ( 'NONE',  ( 8.774405178022840701, 41.09117345860662596, 75.37437276336991943 ) ) ;
#16525 = CARTESIAN_POINT ( 'NONE',  ( -4.344504932464894331, 37.57120742909659583, 78.93669174070734584 ) ) ;
#16526 = CARTESIAN_POINT ( 'NONE',  ( -1.579458713576543882, 38.67424504380988282, 95.05433879952670395 ) ) ;
#16527 = CARTESIAN_POINT ( 'NONE',  ( 0.5838098623046882318, 52.35423961828406192, 78.93669174070734584 ) ) ;
#16528 = ORIENTED_EDGE ( 'NONE', *, *, #15594, .T. ) ;
#16529 = EDGE_CURVE ( 'NONE', #12999, #19914, #15684, .T. ) ;
#16530 = CARTESIAN_POINT ( 'NONE',  ( -4.030259451132765847, 50.97805036467345019, 76.44257241107362688 ) ) ;
#16531 = ORIENTED_EDGE ( 'NONE', *, *, #8070, .F. ) ;
#16532 = DIRECTION ( 'NONE',  ( -1.402518428993831183E-16, 1.000000000000000000, -3.469446951953617640E-16 ) ) ;
#16533 = EDGE_CURVE ( 'NONE', #9230, #2058, #5984, .T. ) ;
#16534 = CARTESIAN_POINT ( 'NONE',  ( 2.522153740306506187, 47.62628298661744708, 77.15433879953100416 ) ) ;
#16535 = CARTESIAN_POINT ( 'NONE',  ( -4.225701142979731095, 37.47645191542193999, 77.17835598703557309 ) ) ;
#16536 = CARTESIAN_POINT ( 'NONE',  ( -3.154801521863568325, 47.83913663364972280, 95.05036078214054385 ) ) ;
#16537 = CARTESIAN_POINT ( 'NONE',  ( 1.658154530501163570, 36.04125148601230677, 76.16022115247204738 ) ) ;
#16538 = DIRECTION ( 'NONE',  ( 1.000000000000000000, 1.402518428993831676E-16, 0.000000000000000000 ) ) ;
#16539 = CARTESIAN_POINT ( 'NONE',  ( 5.487461103983354072, 37.64135143674641171, 76.14207271482608519 ) ) ;
#16540 = EDGE_CURVE ( 'NONE', #12382, #17793, #14513, .T. ) ;
#16541 = CARTESIAN_POINT ( 'NONE',  ( -7.600722970659354871, 47.61678050758295200, 78.31366413292410300 ) ) ;
#16542 = ADVANCED_FACE ( 'NONE', ( #12483 ), #7594, .T. ) ;
#16543 = AXIS2_PLACEMENT_3D ( 'NONE', #6889, #2004, #8501 ) ;
#16544 = EDGE_LOOP ( 'NONE', ( #6429, #15254, #4718, #10495 ) ) ;
#16545 = DIRECTION ( 'NONE',  ( 3.893792155548169402E-16, 7.183611964723547524E-17, -1.000000000000000000 ) ) ;
#16546 = CARTESIAN_POINT ( 'NONE',  ( 5.590052860727733552, 36.96774431777176062, 78.26671861549210973 ) ) ;
#16547 = ORIENTED_EDGE ( 'NONE', *, *, #3197, .F. ) ;
#16548 = DIRECTION ( 'NONE',  ( -4.731737692062791983E-17, 0.7071067811865500152, 0.7071067811865451302 ) ) ;
#16549 = CARTESIAN_POINT ( 'NONE',  ( 2.119851040271390819, 52.81592988514039178, 72.45433879953087342 ) ) ;
#16550 = CARTESIAN_POINT ( 'NONE',  ( -3.981178359372548492, 46.76218137147973408, 92.60183879953099506 ) ) ;
#16551 = ORIENTED_EDGE ( 'NONE', *, *, #20250, .T. ) ;
#16552 = CARTESIAN_POINT ( 'NONE',  ( 8.850612593395874583, 41.31957191698789700, 78.01079203130994699 ) ) ;
#16553 = CARTESIAN_POINT ( 'NONE',  ( -4.477846259693498254, 37.66218137147969713, 54.55433879953098852 ) ) ;
#16554 = ORIENTED_EDGE ( 'NONE', *, *, #6245, .F. ) ;
#16555 = CARTESIAN_POINT ( 'NONE',  ( -3.777846259693486974, 51.36218137147968577, 53.35433879953099279 ) ) ;
#16556 = CARTESIAN_POINT ( 'NONE',  ( 0.5968135028669416808, 52.96212007873675276, 76.86006965461024265 ) ) ;
#16557 = ORIENTED_EDGE ( 'NONE', *, *, #8841, .T. ) ;
#16558 = DIRECTION ( 'NONE',  ( 0.000000000000000000, 0.000000000000000000, 1.000000000000000000 ) ) ;
#16559 = VECTOR ( 'NONE', #560, 1000.000000000000000 ) ;
#16560 = VERTEX_POINT ( 'NONE', #13974 ) ;
#16561 = CARTESIAN_POINT ( 'NONE',  ( -4.385738940255031970, 50.72403773668145277, 76.01646854312687651 ) ) ;
#16562 = DIRECTION ( 'NONE',  ( -1.540237394707284220E-16, -1.793354297423764243E-16, 1.000000000000000000 ) ) ;
#16563 = DIRECTION ( 'NONE',  ( 1.000000000000000000, 0.000000000000000000, 0.000000000000000000 ) ) ;
#16564 = EDGE_CURVE ( 'NONE', #5867, #12858, #7483, .T. ) ;
#16565 = CARTESIAN_POINT ( 'NONE',  ( 6.848903495604322877, 50.42928078925980628, 75.87133531663224062 ) ) ;
#16566 = LINE ( 'NONE', #5163, #6793 ) ;
#16567 = CIRCLE ( 'NONE', #13503, 12.75100040032031501 ) ;
#16568 = CARTESIAN_POINT ( 'NONE',  ( -3.168337701141985541, 36.83946597969015357, 78.91793020585129170 ) ) ;
#16569 = CARTESIAN_POINT ( 'NONE',  ( 4.400857426521584514, 36.11798879971178167, 76.47837415541054895 ) ) ;
#16570 = CARTESIAN_POINT ( 'NONE',  ( 8.390051116449676272, 39.93923995310483832, 78.49952087821802138 ) ) ;
#16571 = AXIS2_PLACEMENT_3D ( 'NONE', #528, #7010, #16920 ) ;
#16572 = VERTEX_POINT ( 'NONE', #1205 ) ;
#16573 = FACE_OUTER_BOUND ( 'NONE', #3455, .T. ) ;
#16574 = CARTESIAN_POINT ( 'NONE',  ( 9.064651367107570579, 41.96105970016846243, 75.41143022427675646 ) ) ;
#16575 = CARTESIAN_POINT ( 'NONE',  ( 31.03948732994507864, 45.16218137147969003, 78.30433879953099563 ) ) ;
#16576 = CARTESIAN_POINT ( 'NONE',  ( -7.215762730499807098, 41.44826869547889459, 78.81763548507551320 ) ) ;
#16577 = VERTEX_POINT ( 'NONE', #9305 ) ;
#16578 = ORIENTED_EDGE ( 'NONE', *, *, #5979, .F. ) ;
#16579 = DIRECTION ( 'NONE',  ( 0.3165065846431827645, 0.9485903129789529098, 0.000000000000000000 ) ) ;
#16580 = ORIENTED_EDGE ( 'NONE', *, *, #18103, .F. ) ;
#16581 = CARTESIAN_POINT ( 'NONE',  ( -3.509782604184570776, 36.19999572785945219, 77.03801799112748938 ) ) ;
#16582 = CIRCLE ( 'NONE', #7402, 4.200000000000001066 ) ;
#16583 = EDGE_CURVE ( 'NONE', #10025, #6298, #15990, .T. ) ;
#16584 = CARTESIAN_POINT ( 'NONE',  ( 8.908783915644443496, 41.49391506008672792, 75.36120592425527320 ) ) ;
#16585 = CARTESIAN_POINT ( 'NONE',  ( 4.226735822238441465, 51.44133747523171252, 77.44183710417100031 ) ) ;
#16586 = CARTESIAN_POINT ( 'NONE',  ( -5.389245695702296501, 49.84508174962770255, 75.45433879953088763 ) ) ;
#16587 = CARTESIAN_POINT ( 'NONE',  ( -1.419351766502868761, 49.49642391118513274, 94.75121379782397923 ) ) ;
#16588 = CARTESIAN_POINT ( 'NONE',  ( 0.5867509473165513079, 52.35421642379873930, 77.38375056423674891 ) ) ;
#16589 = LINE ( 'NONE', #3599, #16313 ) ;
#16590 = LINE ( 'NONE', #16386, #5792 ) ;
#16591 = CARTESIAN_POINT ( 'NONE',  ( -3.350035803220276609, 49.20851703305431357, 93.22683880123798872 ) ) ;
#16592 = CARTESIAN_POINT ( 'NONE',  ( 6.198496396448986090, 45.68315280215533392, 94.08621380123798872 ) ) ;
#16593 = VERTEX_POINT ( 'NONE', #12387 ) ;
#16594 = CARTESIAN_POINT ( 'NONE',  ( 0.4466774018966609971, 52.96665978300602262, 75.99769453967874711 ) ) ;
#16595 = VERTEX_POINT ( 'NONE', #17167 ) ;
#16596 = FACE_OUTER_BOUND ( 'NONE', #12101, .T. ) ;
#16597 = CARTESIAN_POINT ( 'NONE',  ( 8.882918921757626762, 41.41639603256331981, 78.93548851266230315 ) ) ;
#16598 = CARTESIAN_POINT ( 'NONE',  ( 8.504176331704195846, 42.28161211148372445, 75.44322627322523545 ) ) ;
#16599 = CARTESIAN_POINT ( 'NONE',  ( -0.3080929418689875576, 37.85583172076933778, 93.85183880123797451 ) ) ;
#16600 = EDGE_CURVE ( 'NONE', #10780, #15934, #4538, .T. ) ;
#16601 = CARTESIAN_POINT ( 'NONE',  ( 8.951667845840693971, 41.62244091939069790, 77.14698585835439815 ) ) ;
#16602 = DIRECTION ( 'NONE',  ( -0.000000000000000000, -0.000000000000000000, 1.000000000000000000 ) ) ;
#16603 = DIRECTION ( 'NONE',  ( 5.731934358295347564E-32, -3.469446951953617147E-16, -1.000000000000000000 ) ) ;
#16604 = VERTEX_POINT ( 'NONE', #2588 ) ;
#16605 = ORIENTED_EDGE ( 'NONE', *, *, #6375, .T. ) ;
#16606 = CARTESIAN_POINT ( 'NONE',  ( 7.956821099345868120, 40.70147494987158154, 79.37917410394513240 ) ) ;
#16607 = LINE ( 'NONE', #19472, #8054 ) ;
#16608 = LINE ( 'NONE', #14793, #10292 ) ;
#16609 = VERTEX_POINT ( 'NONE', #14077 ) ;
#16610 = CARTESIAN_POINT ( 'NONE',  ( 0.5221537403065106275, 40.96218137147968719, 45.55433879953100273 ) ) ;
#16611 = ADVANCED_FACE ( 'NONE', ( #12788 ), #10113, .T. ) ;
#16612 = VECTOR ( 'NONE', #8785, 1000.000000000000000 ) ;
#16613 = CARTESIAN_POINT ( 'NONE',  ( -4.705149740856862550, 37.08296527939383935, 78.93669174070734584 ) ) ;
#16614 = EDGE_CURVE ( 'NONE', #5130, #15999, #8951, .T. ) ;
#16615 = ORIENTED_EDGE ( 'NONE', *, *, #1866, .F. ) ;
#16616 = CARTESIAN_POINT ( 'NONE',  ( -5.058133621542618030, 44.89684013992257405, 94.24246380294498238 ) ) ;
#16617 = CARTESIAN_POINT ( 'NONE',  ( 2.105044654678958960, 52.94034470533341619, 77.53128952716078004 ) ) ;
#16618 = B_SPLINE_CURVE_WITH_KNOTS ( 'NONE', 3,
 ( #2229, #9044, #8829, #10760, #9154, #4023, #10549, #625, #7106, #17016, #13820, #12235, #20086, #18719, #5523, #948, #4132, #12444, #15645, #736, #17125, #7219, #4340, #2548, #13719, #15532, #1062 ),
 .UNSPECIFIED., .F., .F.,
 ( 4, 1, 1, 1, 1, 1, 1, 1, 1, 1, 1, 1, 1, 1, 1, 1, 1, 1, 1, 1, 1, 1, 1, 1, 4 ),
 ( 0.000000000000000000, 0.05524556061070538121, 0.1069179814647366472, 0.1553727729060086771, 0.2000758033479648479, 0.2417614041178833273, 0.2799066487053696317, 0.3152370222690974444, 0.3476361288249658066, 0.3788200842211088548, 0.4103815830948299714, 0.4425365161269811387, 0.4758329365342930384, 0.5105782220665333604, 0.5468313811506283484, 0.5849849847693828764, 0.6253480228319793222, 0.6671656491570584491, 0.7102157423341657339, 0.7546653220675233475, 0.8003710923354008244, 0.8474641787091774514, 0.8966644363699035614, 0.9474646149202431422, 1.000000000000000000 ),
 .UNSPECIFIED. ) ;
#16619 = CARTESIAN_POINT ( 'NONE',  ( 1.352400422481993658, 50.46853102219002096, 95.57058880123798872 ) ) ;
#16620 = LINE ( 'NONE', #14905, #5482 ) ;
#16621 = ORIENTED_EDGE ( 'NONE', *, *, #5323, .T. ) ;
#16622 = FACE_OUTER_BOUND ( 'NONE', #6665, .T. ) ;
#16623 = VECTOR ( 'NONE', #19810, 1000.000000000000114 ) ;
#16624 = VERTEX_POINT ( 'NONE', #11270 ) ;
#16625 = CARTESIAN_POINT ( 'NONE',  ( 0.5221537403065017457, 49.16218137147969003, 92.45433879953097289 ) ) ;
#16626 = CARTESIAN_POINT ( 'NONE',  ( 5.611423337425062385, 41.22389019960463230, 95.17996380123798872 ) ) ;
#16627 =( BOUNDED_CURVE ( )  B_SPLINE_CURVE ( 2, ( #6359, #7973, #11493, #10003, #17965 ),
 .UNSPECIFIED., .F., .F. ) 
 B_SPLINE_CURVE_WITH_KNOTS ( ( 3, 2, 3 ),
 ( 0.3212199771556245032, 0.3385307364581348621, 0.3472607999482700269 ),
 .UNSPECIFIED. ) 
 CURVE ( )  GEOMETRIC_REPRESENTATION_ITEM ( )  RATIONAL_B_SPLINE_CURVE ( ( 0.9660722070856944121, 0.9493985675917804290, 1.000000000000000000, 0.9744809739482959143, 0.9660722130358361248 ) ) 
 REPRESENTATION_ITEM ( '' )  );
#16628 = EDGE_LOOP ( 'NONE', ( #11310, #7179, #11519, #11619, #8886, #17956, #7867, #2911, #12703, #15882, #5260, #19446 ) ) ;
#16629 = CARTESIAN_POINT ( 'NONE',  ( 8.405094150187295554, 41.90291579521269227, 78.13275527786953489 ) ) ;
#16630 = CARTESIAN_POINT ( 'NONE',  ( 7.992842972995377160, 41.12996670827969581, 75.40210940951681096 ) ) ;
#16632 = AXIS2_PLACEMENT_3D ( 'NONE', #2858, #4643, #21017 ) ;
#16631 = DIRECTION ( 'NONE',  ( -0.5941461771851692664, -0.8043570849667761591, -2.357623395011396791E-16 ) ) ;
#16633 = CARTESIAN_POINT ( 'NONE',  ( 10.77494014480653561, 42.96218137147968008, 65.80574467885102763 ) ) ;
#16634 = CARTESIAN_POINT ( 'NONE',  ( 0.3955195401054462656, 52.96707764484158787, 78.86056079792015794 ) ) ;
#16635 = ORIENTED_EDGE ( 'NONE', *, *, #12875, .T. ) ;
#16636 = CARTESIAN_POINT ( 'NONE',  ( -4.592862224480082745, 51.32295045326189609, 75.97198585835440099 ) ) ;
#16637 = VECTOR ( 'NONE', #18353, 1000.000000000000000 ) ;
#16638 = EDGE_CURVE ( 'NONE', #7250, #14796, #16051, .T. ) ;
#16639 = ORIENTED_EDGE ( 'NONE', *, *, #3001, .F. ) ;
#16640 = CARTESIAN_POINT ( 'NONE',  ( -3.431593788640828535, 36.97795561491845007, 77.76122236671984922 ) ) ;
#16641 = CARTESIAN_POINT ( 'NONE',  ( -7.496610734713931912, 40.31662449841055462, 77.72888818034803649 ) ) ;
#16642 = AXIS2_PLACEMENT_3D ( 'NONE', #6973, #1892, #11588 ) ;
#16643 = FACE_OUTER_BOUND ( 'NONE', #20068, .T. ) ;
#16644 = CARTESIAN_POINT ( 'NONE',  ( 5.220616844236031007, 45.87228208810806507, 92.48558879611698558 ) ) ;
#16645 = CARTESIAN_POINT ( 'NONE',  ( 2.921181103050038086, 49.30691215337508737, 94.59496379782397923 ) ) ;
#16646 = VECTOR ( 'NONE', #13969, 1000.000000000000114 ) ;
#16647 = ORIENTED_EDGE ( 'NONE', *, *, #18945, .F. ) ;
#16648 = LINE ( 'NONE', #5036, #4386 ) ;
#16649 = CARTESIAN_POINT ( 'NONE',  ( 5.388220764666090012, 37.58132116110721199, 78.33482135361461474 ) ) ;
#16650 = EDGE_CURVE ( 'NONE', #2739, #10557, #13767, .T. ) ;
#16651 = ORIENTED_EDGE ( 'NONE', *, *, #11333, .T. ) ;
#16652 = DIRECTION ( 'NONE',  ( -2.267473790562806355E-16, 5.922860397471811774E-17, -1.000000000000000000 ) ) ;
#16653 = EDGE_CURVE ( 'NONE', #4876, #14294, #4205, .T. ) ;
#16654 = LINE ( 'NONE', #13145, #15706 ) ;
#16655 = CARTESIAN_POINT ( 'NONE',  ( -2.904223097202481174, 48.62752260303690122, 93.77371379953099506 ) ) ;
#16656 = AXIS2_PLACEMENT_3D ( 'NONE', #13423, #752, #13210 ) ;
#16657 = EDGE_LOOP ( 'NONE', ( #9765, #6979, #4931, #11280 ) ) ;
#16658 = VECTOR ( 'NONE', #5326, 1000.000000000000114 ) ;
#16659 = CARTESIAN_POINT ( 'NONE',  ( -4.709702680700027955, 38.02233484874552261, 75.39928922905468767 ) ) ;
#16660 = ORIENTED_EDGE ( 'NONE', *, *, #1771, .F. ) ;
#16661 = CARTESIAN_POINT ( 'NONE',  ( 8.832380548758539618, 43.45507459029313679, 75.00433879953099847 ) ) ;
#16662 = CARTESIAN_POINT ( 'NONE',  ( -4.156729428781747337, 37.43250522858453877, 76.44623874561141008 ) ) ;
#16663 = EDGE_CURVE ( 'NONE', #16858, #5644, #17832, .T. ) ;
#16664 = ADVANCED_FACE ( 'NONE', ( #12648 ), #12117, .T. ) ;
#16665 = ORIENTED_EDGE ( 'NONE', *, *, #20787, .T. ) ;
#16666 = PLANE ( 'NONE',  #18695 ) ;
#16667 = CIRCLE ( 'NONE', #7489, 6.000000000000002665 ) ;
#16668 = ORIENTED_EDGE ( 'NONE', *, *, #4652, .F. ) ;
#16669 = CARTESIAN_POINT ( 'NONE',  ( -4.804273704418943858, 51.17188354996588373, 76.37148643835737971 ) ) ;
#16670 = CARTESIAN_POINT ( 'NONE',  ( 2.054490523354237208, 52.82782863985672606, 76.04066109323893841 ) ) ;
#16671 = ADVANCED_FACE ( 'NONE', ( #16277 ), #4463, .F. ) ;
#16672 = SHAPE_REPRESENTATION_RELATIONSHIP ( 'NONE' , 'NONE' ,  #333, #2752 ) ;
#16673 = CARTESIAN_POINT ( 'NONE',  ( 6.398363615859712361, 50.76207644957375464, 75.46588380158773646 ) ) ;
#16674 = AXIS2_PLACEMENT_3D ( 'NONE', #18157, #3577, #8273 ) ;
#16675 = CARTESIAN_POINT ( 'NONE',  ( 5.574863508716481064, 50.62051970816712299, 77.07851092216984057 ) ) ;
#16676 = LINE ( 'NONE', #16779, #7553 ) ;
#16677 = CARTESIAN_POINT ( 'NONE',  ( 3.958912314344054550, 36.72196658547137815, 76.73963291717792856 ) ) ;
#16678 = CARTESIAN_POINT ( 'NONE',  ( 8.515342467852711650, 40.31474608159486195, 79.26294543469528264 ) ) ;
#16679 = VECTOR ( 'NONE', #1499, 1000.000000000000000 ) ;
#16680 = VERTEX_POINT ( 'NONE', #13086 ) ;
#16681 = CARTESIAN_POINT ( 'NONE',  ( -0.9435709597102902579, 52.23013218523595214, 78.24716094272973521 ) ) ;
#16682 = DIRECTION ( 'NONE',  ( -1.000000000000000000, 0.000000000000000000, 0.000000000000000000 ) ) ;
#16683 = CARTESIAN_POINT ( 'NONE',  ( -4.567115856812060670, 47.10047254335474065, 93.46121380123797451 ) ) ;
#16684 = VERTEX_POINT ( 'NONE', #7984 ) ;
#16685 = VERTEX_POINT ( 'NONE', #1708 ) ;
#16686 = EDGE_CURVE ( 'NONE', #4858, #1116, #8451, .T. ) ;
#16687 = DIRECTION ( 'NONE',  ( -1.540237394707284220E-16, -1.793354297423764243E-16, 1.000000000000000000 ) ) ;
#16688 = EDGE_LOOP ( 'NONE', ( #12165, #20594, #304, #1244, #11190, #15322, #14538, #6176, #7575, #250, #11253, #18849 ) ) ;
#16689 = FACE_OUTER_BOUND ( 'NONE', #20135, .T. ) ;
#16690 = CARTESIAN_POINT ( 'NONE',  ( -1.477846259693489372, 49.81903562097208038, 53.15433879953100416 ) ) ;
#16691 = CARTESIAN_POINT ( 'NONE',  ( -3.004571163435685310, 37.81598267955332915, 77.68963291717793140 ) ) ;
#16692 = LINE ( 'NONE', #2006, #14360 ) ;
#16693 = PLANE ( 'NONE',  #10335 ) ;
#16694 = B_SPLINE_SURFACE_WITH_KNOTS ( 'NONE', 3, 1, ( 
 ( #13889, #12511 ),
 ( #20372, #10930 ),
 ( #17401, #15817 ),
 ( #5918, #11133 ),
 ( #17295, #20784 ),
 ( #15714, #12718 ),
 ( #15605, #2827 ),
 ( #7620, #2617 ),
 ( #5806, #14102 ),
 ( #18792, #1229 ),
 ( #1132, #20584 ),
 ( #7720, #1021 ),
 ( #6218, #12616 ),
 ( #12415, #14200 ),
 ( #4513, #14001 ),
 ( #10731, #10831 ),
 ( #17502, #4207 ),
 ( #19103, #20678 ),
 ( #20484, #2926 ) ),
 .UNSPECIFIED., .F., .F., .F.,
 ( 4, 1, 1, 1, 1, 1, 1, 1, 1, 1, 1, 1, 1, 1, 1, 1, 4 ),
 ( 2, 2 ),
 ( 0.000000000000000000, 0.1068357064626556524, 0.2062857352809531475, 0.2975635024103033266, 0.3806658168942347320, 0.4556695234475648948, 0.5225582867794639208, 0.5822950421180911329, 0.6340416422721021350, 0.6795378779249960921, 0.7218021178892558565, 0.7627433693661896941, 0.8042009657065650741, 0.8472253578321278233, 0.8932235139329930407, 0.9440217631200717996, 0.9999999999999998890 ),
 ( 0.000000000000000000, 1.000000000000000000 ),
 .UNSPECIFIED. ) ;
#16695 = CARTESIAN_POINT ( 'NONE',  ( 8.240650035186204647, 41.41153111371846762, 76.01674029036281866 ) ) ;
#16696 = CARTESIAN_POINT ( 'NONE',  ( -1.218186307993492257, 38.53589529967373295, 92.55433879953098142 ) ) ;
#16697 = FACE_OUTER_BOUND ( 'NONE', #11044, .T. ) ;
#16698 = CARTESIAN_POINT ( 'NONE',  ( 5.243738908420800371, 37.46719647903651662, 77.75916469768418438 ) ) ;
#16699 = CARTESIAN_POINT ( 'NONE',  ( 6.828503391016846891, 43.33193468930419101, 92.75808880123800293 ) ) ;
#16700 = CARTESIAN_POINT ( 'NONE',  ( 0.5221537403065006355, 44.16218137147969003, 92.45433879953097289 ) ) ;
#16701 = EDGE_LOOP ( 'NONE', ( #3261, #10280, #6150, #14382 ) ) ;
#16702 = CARTESIAN_POINT ( 'NONE',  ( 0.5245867512892138373, 52.35470670054147035, 75.97350791242078571 ) ) ;
#16703 = CIRCLE ( 'NONE', #13639, 8.199999999999995737 ) ;
#16704 = VERTEX_POINT ( 'NONE', #2881 ) ;
#16705 = CARTESIAN_POINT ( 'NONE',  ( -4.699348147190204550, 37.07867987585472491, 75.97299512023676016 ) ) ;
#16706 = LINE ( 'NONE', #420, #4464 ) ;
#16707 = CARTESIAN_POINT ( 'NONE',  ( -4.470581213684321042, 37.66433489937099210, 78.89646723195187406 ) ) ;
#16708 = CARTESIAN_POINT ( 'NONE',  ( -3.350035803220276609, 49.20851703305431357, 94.63308880123798872 ) ) ;
#16709 = CARTESIAN_POINT ( 'NONE',  ( -4.900087432442488122, 37.22695789959892920, 77.32461911834714385 ) ) ;
#16710 = DIRECTION ( 'NONE',  ( 3.154042683594179442E-15, -3.469446951953613203E-16, -1.000000000000000000 ) ) ;
#16711 = CARTESIAN_POINT ( 'NONE',  ( 5.884818748728627646, 51.14141135607439992, 78.06587361566768379 ) ) ;
#16712 = ORIENTED_EDGE ( 'NONE', *, *, #18315, .F. ) ;
#16713 = VERTEX_POINT ( 'NONE', #9481 ) ;
#16714 = CIRCLE ( 'NONE', #1414, 8.199999999999995737 ) ;
#16715 = CARTESIAN_POINT ( 'NONE',  ( 6.482969723869566714, 49.79324824044548592, 77.22012844410386379 ) ) ;
#16716 = CARTESIAN_POINT ( 'NONE',  ( 5.722153740306498371, 44.16218137147968292, 94.58161078214052964 ) ) ;
#16717 = DIRECTION ( 'NONE',  ( 0.3165065846431826535, 0.9485903129789529098, 2.188653791613874008E-16 ) ) ;
#16718 = ORIENTED_EDGE ( 'NONE', *, *, #11073, .T. ) ;
#16719 = AXIS2_PLACEMENT_3D ( 'NONE', #2228, #3706, #10338 ) ;
#16720 = CARTESIAN_POINT ( 'NONE',  ( -4.531772010406379003, 45.91993734822838036, 95.05433879953099563 ) ) ;
#16721 = DIRECTION ( 'NONE',  ( 0.007885122365275663500, 0.9999689119394085113, 1.805443505845543142E-16 ) ) ;
#16722 = CARTESIAN_POINT ( 'NONE',  ( -3.981178359372548492, 46.76218137147973408, 91.66433880294496817 ) ) ;
#16723 = EDGE_CURVE ( 'NONE', #15169, #8316, #2848, .T. ) ;
#16724 = CARTESIAN_POINT ( 'NONE',  ( 2.082493151224042549, 52.94052253222597670, 77.39871602076138402 ) ) ;
#16725 = CARTESIAN_POINT ( 'NONE',  ( 6.828503391016846891, 43.33193468930419101, 94.00808880123798872 ) ) ;
#16726 = VECTOR ( 'NONE', #17533, 1000.000000000000114 ) ;
#16727 = CARTESIAN_POINT ( 'NONE',  ( -7.885657102084565828, 41.56435211639550431, 79.54845644658969661 ) ) ;
#16728 = ORIENTED_EDGE ( 'NONE', *, *, #920, .F. ) ;
#16729 = VECTOR ( 'NONE', #16739, 1000.000000000000000 ) ;
#16730 = CARTESIAN_POINT ( 'NONE',  ( 31.22215374030650281, 42.76218137147968434, 73.80433879953100984 ) ) ;
#16731 = ORIENTED_EDGE ( 'NONE', *, *, #8184, .F. ) ;
#16732 = CARTESIAN_POINT ( 'NONE',  ( -7.694987716518704168, 47.31164717387682828, 78.21926933574907537 ) ) ;
#16733 = CARTESIAN_POINT ( 'NONE',  ( 3.460444912181559474, 49.25145096859824889, 90.49246380123798872 ) ) ;
#16734 = ORIENTED_EDGE ( 'NONE', *, *, #8972, .T. ) ;
#16735 = CARTESIAN_POINT ( 'NONE',  ( 1.964251312053305165, 36.08998497932209659, 72.45433879953085921 ) ) ;
#16736 = CARTESIAN_POINT ( 'NONE',  ( 5.722153740305851777, 42.76884557083668881, 94.52737681315549878 ) ) ;
#16737 = CARTESIAN_POINT ( 'NONE',  ( -4.104527287216266807, 50.75212113806905023, 79.54777180229389444 ) ) ;
#16738 = LINE ( 'NONE', #7255, #10489 ) ;
#16739 = DIRECTION ( 'NONE',  ( -1.000000000000000000, -1.213411507412056509E-16, 0.000000000000000000 ) ) ;
#16740 = VERTEX_POINT ( 'NONE', #17548 ) ;
#16741 = CARTESIAN_POINT ( 'NONE',  ( 4.004906909697989015, 36.73854140438177041, 77.43080938776617472 ) ) ;
#16742 = VECTOR ( 'NONE', #3432, 1000.000000000000114 ) ;
#16743 = ORIENTED_EDGE ( 'NONE', *, *, #9499, .T. ) ;
#16744 = CARTESIAN_POINT ( 'NONE',  ( -3.541825984438901731, 47.99675089776317805, 95.05433879953095300 ) ) ;
#16745 = VECTOR ( 'NONE', #5274, 1000.000000000000227 ) ;
#16746 = CARTESIAN_POINT ( 'NONE',  ( -7.056725745502300029, 41.40963693795823275, 76.59276269229415846 ) ) ;
#16747 = EDGE_CURVE ( 'NONE', #15667, #17279, #2975, .T. ) ;
#16748 = DIRECTION ( 'NONE',  ( -0.000000000000000000, -0.000000000000000000, 1.000000000000000000 ) ) ;
#16749 = CARTESIAN_POINT ( 'NONE',  ( 6.853523395152754105, 50.42586825556427499, 78.95155228521747404 ) ) ;
#16750 = EDGE_CURVE ( 'NONE', #2871, #14563, #1386, .T. ) ;
#16751 = CARTESIAN_POINT ( 'NONE',  ( 6.660594192354429843, 43.89417127335556046, 94.36058879782399345 ) ) ;
#16752 = CARTESIAN_POINT ( 'NONE',  ( 5.471586674567812558, 37.63000815068602378, 76.06531707679772580 ) ) ;
#16753 = ORIENTED_EDGE ( 'NONE', *, *, #3034, .T. ) ;
#16754 = CARTESIAN_POINT ( 'NONE',  ( 3.117507734380600581, 51.94062193790708903, 75.45433879953088763 ) ) ;
#16755 = ORIENTED_EDGE ( 'NONE', *, *, #17674, .F. ) ;
#16756 = B_SPLINE_CURVE_WITH_KNOTS ( 'NONE', 3,
 ( #10071, #11870, #8574, #18349, #16552, #13361, #19831, #18243, #16763, #20038, #3664 ),
 .UNSPECIFIED., .F., .F.,
 ( 4, 1, 1, 1, 1, 1, 1, 1, 4 ),
 ( 0.000000000000000000, 0.1094333067106434410, 0.2184679721593839052, 0.3300813608894926365, 0.4462978032959263319, 0.5702501687912749917, 0.7022991718047063570, 0.8456887798043180027, 0.9999999999999998890 ),
 .UNSPECIFIED. ) ;
#16757 = DIRECTION ( 'NONE',  ( -1.540237394707284467E-16, -1.793354297423764243E-16, 1.000000000000000000 ) ) ;
#16758 = EDGE_CURVE ( 'NONE', #11489, #6337, #17767, .T. ) ;
#16759 = CARTESIAN_POINT ( 'NONE',  ( 3.948530577815480225, 39.69684013992245752, 93.14871379953099506 ) ) ;
#16760 = CARTESIAN_POINT ( 'NONE',  ( 5.544968037009670780, 45.50804040601273925, 92.13308879953099506 ) ) ;
#16761 = CARTESIAN_POINT ( 'NONE',  ( -7.191377436723248806, 41.79953674621017257, 77.84082762752957763 ) ) ;
#16762 = ORIENTED_EDGE ( 'NONE', *, *, #1300, .T. ) ;
#16763 = CARTESIAN_POINT ( 'NONE',  ( 8.985665979147935190, 41.72433548171385098, 78.13399373581940210 ) ) ;
#16764 = CARTESIAN_POINT ( 'NONE',  ( 24.52215374030649642, 44.16218137147969003, 87.85433879953103542 ) ) ;
#16765 = ORIENTED_EDGE ( 'NONE', *, *, #9650, .F. ) ;
#16766 = CARTESIAN_POINT ( 'NONE',  ( 1.233827257842946334, 39.01589007119768837, 95.05433879953096721 ) ) ;
#16767 = LINE ( 'NONE', #13262, #17996 ) ;
#16768 = ORIENTED_EDGE ( 'NONE', *, *, #13310, .T. ) ;
#16769 = CARTESIAN_POINT ( 'NONE',  ( 1.690580188175442533, 52.27889548997219293, 79.31285334339766280 ) ) ;
#16770 = ORIENTED_EDGE ( 'NONE', *, *, #19848, .F. ) ;
#16771 = CARTESIAN_POINT ( 'NONE',  ( 0.6935063668540784043, 52.36041438938426040, 77.40588291575248547 ) ) ;
#16772 = DIRECTION ( 'NONE',  ( 1.402518428993831676E-16, -1.000000000000000000, 0.000000000000000000 ) ) ;
#16773 = EDGE_CURVE ( 'NONE', #8766, #2112, #4097, .T. ) ;
#16774 = EDGE_CURVE ( 'NONE', #13434, #18535, #8794, .T. ) ;
#16775 = ADVANCED_FACE ( 'NONE', ( #13190 ), #16877, .F. ) ;
#16776 = VECTOR ( 'NONE', #7421, 1000.000000000000000 ) ;
#16777 = CARTESIAN_POINT ( 'NONE',  ( -4.887610060180215932, 37.21774136732800997, 76.16751655709613544 ) ) ;
#16778 = CARTESIAN_POINT ( 'NONE',  ( 5.220616844236030119, 45.87228208810806507, 94.04808879953097289 ) ) ;
#16779 = CARTESIAN_POINT ( 'NONE',  ( 5.427780505986065762, 36.85179043424346190, 77.43080938776617472 ) ) ;
#16780 = ORIENTED_EDGE ( 'NONE', *, *, #15869, .F. ) ;
#16781 = EDGE_CURVE ( 'NONE', #12015, #9638, #4980, .T. ) ;
#16782 = CARTESIAN_POINT ( 'NONE',  ( 4.007614759266367344, 36.75676756950254287, 76.14998054923410109 ) ) ;
#16783 = B_SPLINE_CURVE_WITH_KNOTS ( 'NONE', 3,
 ( #857, #20205, #12144, #15440, #3721, #18624, #3934, #18415, #16924, #5538, #11827 ),
 .UNSPECIFIED., .F., .F.,
 ( 4, 1, 1, 1, 1, 1, 1, 1, 4 ),
 ( 0.000000000000000000, 0.2026380577750736822, 0.3699241180509920679, 0.5036394156482512097, 0.6074627879459471025, 0.6969630674522783176, 0.7888943515530689732, 0.8885774882565341537, 1.000000000000000000 ),
 .UNSPECIFIED. ) ;
#16784 = VERTEX_POINT ( 'NONE', #15398 ) ;
#16785 = LINE ( 'NONE', #18479, #11894 ) ;
#16786 = DIRECTION ( 'NONE',  ( -0.3014928876834147564, 0.9534151938875496946, -0.01007505536868189694 ) ) ;
#16787 = PLANE ( 'NONE',  #10964 ) ;
#16788 = ORIENTED_EDGE ( 'NONE', *, *, #13526, .T. ) ;
#16789 = ORIENTED_EDGE ( 'NONE', *, *, #18627, .F. ) ;
#16790 = AXIS2_PLACEMENT_3D ( 'NONE', #10906, #12485, #2906 ) ;
#16791 = CARTESIAN_POINT ( 'NONE',  ( 6.374498485212880539, 49.86568965500833883, 79.04700635913849283 ) ) ;
#16792 = ORIENTED_EDGE ( 'NONE', *, *, #1588, .T. ) ;
#16793 = CARTESIAN_POINT ( 'NONE',  ( -3.495943983152252965, 36.18977369595653926, 76.77671532909576513 ) ) ;
#16794 = CARTESIAN_POINT ( 'NONE',  ( 6.774925554820337759, 37.81441096401221102, 75.87985893138584004 ) ) ;
#16795 = DIRECTION ( 'NONE',  ( 0.8136266022444372803, 0.5813877811927012917, 2.295812393977109100E-16 ) ) ;
#16796 = CARTESIAN_POINT ( 'NONE',  ( 4.098112526425296664, 51.53634632258648907, 76.74217282813371810 ) ) ;
#16797 = DIRECTION ( 'NONE',  ( 0.3165065846431827645, 0.9485903129789529098, 0.000000000000000000 ) ) ;
#16798 = CARTESIAN_POINT ( 'NONE',  ( 8.787829143201872029, 41.13140593384864729, 78.45948585835439815 ) ) ;
#16799 = CARTESIAN_POINT ( 'NONE',  ( 0.8446148313103564176, 52.35218307230691437, 77.70257284945761000 ) ) ;
#16800 = FACE_OUTER_BOUND ( 'NONE', #20774, .T. ) ;
#16801 = CARTESIAN_POINT ( 'NONE',  ( 4.169442455018850247, 51.48365777767921969, 75.94315254166910734 ) ) ;
#16802 = ADVANCED_FACE ( 'NONE', ( #18575 ), #2077, .F. ) ;
#16803 = CARTESIAN_POINT ( 'NONE',  ( -0.8237052942265477018, 49.18499566818285018, 95.25808880294498238 ) ) ;
#16804 = CARTESIAN_POINT ( 'NONE',  ( 8.378499831177387946, 41.81317597918418016, 76.33673353730570454 ) ) ;
#16805 = ORIENTED_EDGE ( 'NONE', *, *, #4411, .T. ) ;
#16806 = EDGE_CURVE ( 'NONE', #4528, #4917, #200, .T. ) ;
#16807 = CARTESIAN_POINT ( 'NONE',  ( 0.5548452009814999197, 52.35446810154547848, 75.97250646058495249 ) ) ;
#16808 = EDGE_CURVE ( 'NONE', #2288, #559, #8186, .T. ) ;
#16809 = VERTEX_POINT ( 'NONE', #17601 ) ;
#16810 = CARTESIAN_POINT ( 'NONE',  ( -4.718161399584266391, 37.09257646755418847, 75.97198585835440099 ) ) ;
#16811 = CARTESIAN_POINT ( 'NONE',  ( 23.03948732994508575, 43.16218137147969003, 78.60433879953099279 ) ) ;
#16812 = CARTESIAN_POINT ( 'NONE',  ( 8.618999050077414736, 42.86439581318003178, 75.78893996921105725 ) ) ;
#16813 = CARTESIAN_POINT ( 'NONE',  ( -0.9988176903691428077, 49.83852402762217082, 95.80496380123798872 ) ) ;
#16814 = DIRECTION ( 'NONE',  ( 1.540237394707283727E-16, 1.793354297423763257E-16, -1.000000000000000000 ) ) ;
#16815 = LINE ( 'NONE', #10233, #3822 ) ;
#16816 = CARTESIAN_POINT ( 'NONE',  ( -3.350035803220276609, 49.20851703305431357, 90.88308880123797451 ) ) ;
#16817 = CARTESIAN_POINT ( 'NONE',  ( 5.425723373820400930, 50.72741113942812063, 77.95070864408322109 ) ) ;
#16818 = VERTEX_POINT ( 'NONE', #9331 ) ;
#16819 = VERTEX_POINT ( 'NONE', #7513 ) ;
#16820 = CARTESIAN_POINT ( 'NONE',  ( 8.990918003704509331, 41.74007613249212767, 79.53018343098241871 ) ) ;
#16821 = DIRECTION ( 'NONE',  ( -0.5800177190770277047, -0.8146038580541355989, -2.354238310054624259E-16 ) ) ;
#16822 = CARTESIAN_POINT ( 'NONE',  ( -4.221808390846331527, 37.47367089672861340, 78.89427195578772967 ) ) ;
#16823 = ORIENTED_EDGE ( 'NONE', *, *, #19132, .F. ) ;
#16824 = CARTESIAN_POINT ( 'NONE',  ( 27.63948732994508006, 43.16218137147969003, 76.90433879953101837 ) ) ;
#16825 = CARTESIAN_POINT ( 'NONE',  ( -4.942049829789907811, 43.24669937789425234, 95.05433879953095300 ) ) ;
#16826 = LINE ( 'NONE', #8743, #9197 ) ;
#16827 = CARTESIAN_POINT ( 'NONE',  ( 3.122153740306552905, 48.66551347115873227, 93.85183880294498238 ) ) ;
#16828 = CARTESIAN_POINT ( 'NONE',  ( 2.000053588515297243, 52.94117259847497792, 77.17808573571203112 ) ) ;
#16829 = CARTESIAN_POINT ( 'NONE',  ( -3.166333418787979248, 36.86031865481220393, 78.01078865174693533 ) ) ;
#16830 = ADVANCED_FACE ( 'NONE', ( #1441 ), #16694, .T. ) ;
#16831 = CARTESIAN_POINT ( 'NONE',  ( 6.828503391016846891, 43.33193468930419101, 95.25808880123800293 ) ) ;
#16832 = CARTESIAN_POINT ( 'NONE',  ( -8.071517288156909942, 42.25946119754487995, 79.44950456819475448 ) ) ;
#16833 = ORIENTED_EDGE ( 'NONE', *, *, #11967, .F. ) ;
#16834 = CARTESIAN_POINT ( 'NONE',  ( 2.122153740306496505, 49.76218137147968434, 69.55433879953100984 ) ) ;
#16835 = VERTEX_POINT ( 'NONE', #18893 ) ;
#16836 = CARTESIAN_POINT ( 'NONE',  ( 0.5221537403065015237, 44.16218137147968292, 75.45433879953088763 ) ) ;
#16837 = CARTESIAN_POINT ( 'NONE',  ( -5.154188915835984375, 42.64120994080404614, 93.46121380123797451 ) ) ;
#16838 = ORIENTED_EDGE ( 'NONE', *, *, #14440, .T. ) ;
#16839 = CARTESIAN_POINT ( 'NONE',  ( 2.228068668033876154, 49.81017696809242778, 92.55433879953098142 ) ) ;
#16840 = LINE ( 'NONE', #7357, #6059 ) ;
#16841 = CARTESIAN_POINT ( 'NONE',  ( -3.118414543444179010, 51.45676120087671279, 79.13154374754441278 ) ) ;
#16842 = CARTESIAN_POINT ( 'NONE',  ( -1.677846259693482001, 44.16218137147969003, 56.15433879953099705 ) ) ;
#16843 = CARTESIAN_POINT ( 'NONE',  ( 0.8440572370183208051, 52.35217469777130361, 76.31365475201417325 ) ) ;
#16844 = CARTESIAN_POINT ( 'NONE',  ( 28.52215374030649642, 44.16218137147969003, 87.85433879953103542 ) ) ;
#16845 = VERTEX_POINT ( 'NONE', #19196 ) ;
#16846 = DIRECTION ( 'NONE',  ( 5.626130192357176673E-16, 1.809130530872730902E-30, -1.000000000000000000 ) ) ;
#16847 = ORIENTED_EDGE ( 'NONE', *, *, #9856, .T. ) ;
#16848 = EDGE_CURVE ( 'NONE', #9648, #7336, #4305, .T. ) ;
#16849 = CARTESIAN_POINT ( 'NONE',  ( 5.037341483232629535, 37.31725042616477594, 72.45433879953087342 ) ) ;
#16850 = CARTESIAN_POINT ( 'NONE',  ( 6.616107328214575034, 50.60123794050897317, 77.65065976741861675 ) ) ;
#16851 = DIRECTION ( 'NONE',  ( -0.3165065846431827645, -0.9485903129789529098, 0.000000000000000000 ) ) ;
#16852 = CARTESIAN_POINT ( 'NONE',  ( 5.483018176437226998, 37.63302714415535632, 76.07972420133452829 ) ) ;
#16853 = CARTESIAN_POINT ( 'NONE',  ( 6.660594192354429843, 43.89417127335556046, 92.01683879782399345 ) ) ;
#16854 = CARTESIAN_POINT ( 'NONE',  ( 8.474591150375477611, 46.20736444405172705, 75.44552964019689512 ) ) ;
#16855 = CARTESIAN_POINT ( 'NONE',  ( -4.652687709939232086, 51.28020135170361016, 75.36022115247205022 ) ) ;
#16856 = VERTEX_POINT ( 'NONE', #3030 ) ;
#16857 = CARTESIAN_POINT ( 'NONE',  ( 8.211364901683856132, 41.32396416616596468, 78.49453464888588883 ) ) ;
#16858 = VERTEX_POINT ( 'NONE', #1336 ) ;
#16859 = DIRECTION ( 'NONE',  ( -1.402518428993831183E-16, 1.000000000000000000, 0.000000000000000000 ) ) ;
#16860 = CARTESIAN_POINT ( 'NONE',  ( 3.122153740306552905, 48.66551347115873227, 92.28933879953099506 ) ) ;
#16861 = CARTESIAN_POINT ( 'NONE',  ( -0.8237052942265477018, 49.18499566818285018, 96.19558879953099506 ) ) ;
#16862 = PRODUCT_DEFINITION_SHAPE ( 'NONE', 'NONE',  #14822 ) ;
#16863 = VERTEX_POINT ( 'NONE', #2720 ) ;
#16864 = EDGE_CURVE ( 'NONE', #17901, #667, #18823, .T. ) ;
#16865 = CARTESIAN_POINT ( 'NONE',  ( 30.92220646078100188, 42.96218137147968008, 61.40715055817103263 ) ) ;
#16866 = CARTESIAN_POINT ( 'NONE',  ( -1.598719209087998694, 36.85794301744668644, 72.45432679953087529 ) ) ;
#16867 = ORIENTED_EDGE ( 'NONE', *, *, #755, .T. ) ;
#16868 = DIRECTION ( 'NONE',  ( -0.9534635866061453857, -0.3015081906286223856, -2.009271279954815304E-16 ) ) ;
#16869 = DIRECTION ( 'NONE',  ( -0.9534635866061452747, -0.3015081906286225522, -2.009271279954815797E-16 ) ) ;
#16870 = ORIENTED_EDGE ( 'NONE', *, *, #14354, .T. ) ;
#16871 = CARTESIAN_POINT ( 'NONE',  ( 1.916709343768108864, 52.24291296276840768, 79.11969604467107331 ) ) ;
#16872 = CARTESIAN_POINT ( 'NONE',  ( 5.611423337425062385, 41.22389019960463230, 95.33621380123798872 ) ) ;
#16873 = VERTEX_POINT ( 'NONE', #15915 ) ;
#16874 = FACE_OUTER_BOUND ( 'NONE', #19386, .T. ) ;
#16875 = CARTESIAN_POINT ( 'NONE',  ( 6.828503391016846891, 43.33193468930419101, 90.25808880123800293 ) ) ;
#16876 = CONTEXT_DEPENDENT_SHAPE_REPRESENTATION ( #13887, #7347 ) ;
#16877 = CYLINDRICAL_SURFACE ( 'NONE', #9313, 4.200000000000003730 ) ;
#16878 = ADVANCED_FACE ( 'NONE', ( #16021 ), #3338, .F. ) ;
#16879 = LINE ( 'NONE', #2297, #13307 ) ;
#16880 = DIRECTION ( 'NONE',  ( -1.334402673828310381E-16, -2.168404344970984808E-15, 1.000000000000000000 ) ) ;
#16881 = ORIENTED_EDGE ( 'NONE', *, *, #7694, .T. ) ;
#16882 = CARTESIAN_POINT ( 'NONE',  ( 1.187762653619208075, 52.20882925152060494, 75.41083127720757773 ) ) ;
#16883 = ORIENTED_EDGE ( 'NONE', *, *, #14966, .F. ) ;
#16884 = CARTESIAN_POINT ( 'NONE',  ( -12.18117835937254867, 39.56218137147966019, 45.55433879953098852 ) ) ;
#16885 = CARTESIAN_POINT ( 'NONE',  ( 0.5221537403065015237, 44.16218137147968292, 75.45433879953088763 ) ) ;
#16886 = CARTESIAN_POINT ( 'NONE',  ( -7.269305757963094194, 41.60587264541594976, 78.93240053410227119 ) ) ;
#16887 = ORIENTED_EDGE ( 'NONE', *, *, #5001, .T. ) ;
#16888 = AXIS2_PLACEMENT_3D ( 'NONE', #316, #14, #13101 ) ;
#16889 = CARTESIAN_POINT ( 'NONE',  ( 8.889576793745449734, 46.88836537034026719, 78.73595644658969661 ) ) ;
#16890 = EDGE_LOOP ( 'NONE', ( #1653, #10422, #638, #12642 ) ) ;
#16891 = LINE ( 'NONE', #7086, #9792 ) ;
#16892 = DIRECTION ( 'NONE',  ( 0.5813877811926937422, -0.8136266022444427204, -5.636455622144829957E-17 ) ) ;
#16893 = CARTESIAN_POINT ( 'NONE',  ( 7.835155343763541502, 40.65736687995521237, 75.56834740413086138 ) ) ;
#16894 = CYLINDRICAL_SURFACE ( 'NONE', #6996, 4.200000000000001066 ) ;
#16895 = PLANE ( 'NONE',  #1274 ) ;
#16896 = CARTESIAN_POINT ( 'NONE',  ( -7.340541098479197224, 41.83271662774721733, 79.54689003211581166 ) ) ;
#16897 = CARTESIAN_POINT ( 'NONE',  ( -0.9988176903691428077, 49.83852402762217082, 94.55496380123798872 ) ) ;
#16898 = CARTESIAN_POINT ( 'NONE',  ( 8.213642321612983466, 41.33058728280212080, 76.23356602378127889 ) ) ;
#16899 = CARTESIAN_POINT ( 'NONE',  ( 0.5221537403065364957, 44.16218137147969003, 123.5543387995310098 ) ) ;
#16900 = CARTESIAN_POINT ( 'NONE',  ( 4.500348682233642705, 51.23923067735156422, 75.54250430092201896 ) ) ;
#16901 = CARTESIAN_POINT ( 'NONE',  ( 3.948530577815480225, 39.69684013992245752, 92.21121380294495395 ) ) ;
#16902 = VECTOR ( 'NONE', #18518, 1000.000000000000114 ) ;
#16903 = CARTESIAN_POINT ( 'NONE',  ( -7.677846259693483333, 47.36218137147966445, 45.55433879953098852 ) ) ;
#16904 = CARTESIAN_POINT ( 'NONE',  ( 8.374753614891972120, 41.81346795830285146, 78.59502675972919405 ) ) ;
#16905 = ORIENTED_EDGE ( 'NONE', *, *, #10781, .T. ) ;
#16906 = LINE ( 'NONE', #6904, #655 ) ;
#16907 = FACE_OUTER_BOUND ( 'NONE', #18286, .T. ) ;
#16908 = CARTESIAN_POINT ( 'NONE',  ( -4.567115856812060670, 47.10047254335474065, 94.71121380123797451 ) ) ;
#16909 = EDGE_CURVE ( 'NONE', #4527, #1211, #9999, .T. ) ;
#16910 = CIRCLE ( 'NONE', #3644, 6.200000000000000178 ) ;
#16911 = DIRECTION ( 'NONE',  ( -0.3165065846431827090, -0.9485903129789527988, 0.000000000000000000 ) ) ;
#16912 = DIRECTION ( 'NONE',  ( 1.540237394707284220E-16, 1.793354297423764243E-16, -1.000000000000000000 ) ) ;
#16913 = CARTESIAN_POINT ( 'NONE',  ( 11.22215374030650281, 42.96218137147968008, 74.20433879953100131 ) ) ;
#16914 = EDGE_CURVE ( 'NONE', #17483, #18148, #11345, .T. ) ;
#16915 = FACE_OUTER_BOUND ( 'NONE', #13076, .T. ) ;
#16916 = ORIENTED_EDGE ( 'NONE', *, *, #4402, .T. ) ;
#16917 = AXIS2_PLACEMENT_3D ( 'NONE', #7144, #15249, #2369 ) ;
#16918 = B_SPLINE_CURVE_WITH_KNOTS ( 'NONE', 3,
 ( #4766, #781, #13757, #20228, #14075, #18649, #10595, #20556, #17062, #12481, #18963, #2489, #8983, #15466, #882 ),
 .UNSPECIFIED., .F., .F.,
 ( 4, 1, 1, 1, 1, 1, 1, 1, 1, 1, 1, 1, 4 ),
 ( 0.000000000000000000, 0.1027118292588455328, 0.1981555131143932502, 0.2874887429483043433, 0.3729525961046017413, 0.4183424594053214429, 0.4719402630404010424, 0.5343443080544488799, 0.6066182697135418245, 0.6887512500569755725, 0.7816623524051020677, 0.8855466611608181493, 1.000000000000000000 ),
 .UNSPECIFIED. ) ;
#16919 = CARTESIAN_POINT ( 'NONE',  ( 8.491509432166619575, 42.60773501221702730, 79.34093170394821470 ) ) ;
#16920 = DIRECTION ( 'NONE',  ( -1.000000000000000000, 0.000000000000000000, 0.000000000000000000 ) ) ;
#16921 = ADVANCED_FACE ( 'NONE', ( #19510 ), #8131, .F. ) ;
#16922 = DIRECTION ( 'NONE',  ( -1.540237394707284220E-16, -1.793354297423764243E-16, 1.000000000000000000 ) ) ;
#16923 = CARTESIAN_POINT ( 'NONE',  ( -2.416137431568557314, 39.07291177436112406, 95.02371380123797451 ) ) ;
#16924 = CARTESIAN_POINT ( 'NONE',  ( 5.710003222748535556, 51.27054054311695808, 77.28795170149270177 ) ) ;
#16925 = DIRECTION ( 'NONE',  ( -0.5813877811927011807, 0.8136266022444372803, 5.636455622144619183E-17 ) ) ;
#16926 = DIRECTION ( 'NONE',  ( -1.779391786395883536E-16, -5.922860397471806844E-17, 1.000000000000000000 ) ) ;
#16927 = VECTOR ( 'NONE', #8768, 1000.000000000000000 ) ;
#16928 = CARTESIAN_POINT ( 'NONE',  ( -0.5048357562844464352, 52.90269622882259881, 79.29516791311903035 ) ) ;
#16929 = CARTESIAN_POINT ( 'NONE',  ( -7.073844619497298147, 47.06934724366217182, 78.18191347276355430 ) ) ;
#16930 = CARTESIAN_POINT ( 'NONE',  ( -0.3080929418689875576, 37.85583172076933778, 94.94558880123797451 ) ) ;
#16931 = CARTESIAN_POINT ( 'NONE',  ( 6.837774032321189743, 37.85932018500469809, 76.05683950549904182 ) ) ;
#16932 = ORIENTED_EDGE ( 'NONE', *, *, #13386, .T. ) ;
#16933 = CARTESIAN_POINT ( 'NONE',  ( 5.934652055452926511, 51.10460149980519873, 77.05868164888072158 ) ) ;
#16934 = ORIENTED_EDGE ( 'NONE', *, *, #14063, .T. ) ;
#16935 = FACE_OUTER_BOUND ( 'NONE', #16347, .T. ) ;
#16936 = CARTESIAN_POINT ( 'NONE',  ( -2.077846259693550746, 39.65884927180063357, 94.47683880294496817 ) ) ;
#16937 = ORIENTED_EDGE ( 'NONE', *, *, #12361, .F. ) ;
#16938 = CARTESIAN_POINT ( 'NONE',  ( -4.007890887056451135, 40.01116025973682611, 92.79808879782399345 ) ) ;
#16939 = AXIS2_PLACEMENT_3D ( 'NONE', #12471, #14262, #4574 ) ;
#16940 = DIRECTION ( 'NONE',  ( -0.9999689119394085113, 0.007885122365275831768, -1.526048693634352652E-16 ) ) ;
#16941 = CARTESIAN_POINT ( 'NONE',  ( -4.139232521079847515, 50.72732204858985483, 79.54845644658969661 ) ) ;
#16942 = CARTESIAN_POINT ( 'NONE',  ( 6.531299583006453524, 48.82481648921748274, 72.45433879953087342 ) ) ;
#16943 = CARTESIAN_POINT ( 'NONE',  ( 0.8457719648580424021, 52.35216117651211221, 76.42615000023204175 ) ) ;
#16944 = EDGE_CURVE ( 'NONE', #1211, #2305, #4922, .T. ) ;
#16945 = CARTESIAN_POINT ( 'NONE',  ( 0.5271520053606592038, 52.96603967447732231, 78.93427191990714675 ) ) ;
#16946 = ORIENTED_EDGE ( 'NONE', *, *, #7772, .F. ) ;
#16947 = CARTESIAN_POINT ( 'NONE',  ( 2.722153740306517911, 49.95873206995546667, 56.15433879953099705 ) ) ;
#16948 = VERTEX_POINT ( 'NONE', #18025 ) ;
#16949 = DIRECTION ( 'NONE',  ( -5.731934358295347564E-32, 3.469446951953617147E-16, 1.000000000000000000 ) ) ;
#16950 = CARTESIAN_POINT ( 'NONE',  ( -2.313335635445063154, 37.76218137147968434, 92.03489701350649455 ) ) ;
#16951 = CARTESIAN_POINT ( 'NONE',  ( -7.845278861804691140, 41.41922261456151233, 76.30903472146037814 ) ) ;
#16952 = LINE ( 'NONE', #8670, #1498 ) ;
#16953 = PLANE ( 'NONE',  #14897 ) ;
#16954 = CARTESIAN_POINT ( 'NONE',  ( -1.876873622437040590, 39.01745058958429269, 95.21996379782397923 ) ) ;
#16955 = PLANE ( 'NONE',  #1087 ) ;
#16956 = CIRCLE ( 'NONE', #8806, 8.199999999999995737 ) ;
#16957 = EDGE_LOOP ( 'NONE', ( #6006, #8064, #20362, #4286 ) ) ;
#16958 = CARTESIAN_POINT ( 'NONE',  ( 8.824963465026481657, 41.24269985211446254, 78.91056401563228917 ) ) ;
#16959 = VERTEX_POINT ( 'NONE', #50 ) ;
#16960 = CARTESIAN_POINT ( 'NONE',  ( 33.61275266354798674, 51.36218137147967866, 92.39963826115175038 ) ) ;
#16961 = CARTESIAN_POINT ( 'NONE',  ( -3.981178359372548492, 46.76218137147973408, 93.85183879953099506 ) ) ;
#16962 = CARTESIAN_POINT ( 'NONE',  ( -4.500660556396669065, 42.81632233694663370, 91.50808879953098085 ) ) ;
#16963 = CARTESIAN_POINT ( 'NONE',  ( -7.980074661670381708, 41.84304719859172650, 77.46376836651262465 ) ) ;
#16964 = ORIENTED_EDGE ( 'NONE', *, *, #15096, .T. ) ;
#16965 = CARTESIAN_POINT ( 'NONE',  ( -2.416137431568557314, 39.07291177436112406, 92.52371380123797451 ) ) ;
#16966 = CARTESIAN_POINT ( 'NONE',  ( 0.4220451763538803913, 52.96170309347347427, 77.42739368347497475 ) ) ;
#16967 = CARTESIAN_POINT ( 'NONE',  ( -4.546431600613201951, 41.68282864742221250, 95.05433879953095300 ) ) ;
#16968 = CARTESIAN_POINT ( 'NONE',  ( 0.5221537403065006355, 44.16218137147969003, 92.45433879953097289 ) ) ;
#16969 = ORIENTED_EDGE ( 'NONE', *, *, #18869, .T. ) ;
#16970 = CARTESIAN_POINT ( 'NONE',  ( -5.927888611570137911, 47.57933715648534445, 78.78375056423675460 ) ) ;
#16971 = AXIS2_PLACEMENT_3D ( 'NONE', #4447, #10659, #17014 ) ;
#16972 = ORIENTED_EDGE ( 'NONE', *, *, #2952, .T. ) ;
#16973 = CARTESIAN_POINT ( 'NONE',  ( -4.451329120265561379, 50.67716939545569232, 76.44036821129557779 ) ) ;
#16974 = DIRECTION ( 'NONE',  ( -0.9485903129789495791, 0.3165065846431928120, -8.934458285744765648E-17 ) ) ;
#16975 = AXIS2_PLACEMENT_3D ( 'NONE', #11893, #3788, #10309 ) ;
#16976 = APPLICATION_PROTOCOL_DEFINITION ( 'draft international standard', 'automotive_design', 1998, #19720 ) ;
#16977 = CARTESIAN_POINT ( 'NONE',  ( 0.5221537403065005245, 44.16218137147968292, 82.45433879953087342 ) ) ;
#16978 = CARTESIAN_POINT ( 'NONE',  ( 5.398882651910504649, 50.75441279359508684, 77.28963291717792572 ) ) ;
#16979 = ADVANCED_FACE ( 'NONE', ( #1544 ), #18117, .F. ) ;
#16980 = CARTESIAN_POINT ( 'NONE',  ( -3.140505196763866191, 36.82560845944811945, 78.82932626445051483 ) ) ;
#16981 = ORIENTED_EDGE ( 'NONE', *, *, #1866, .T. ) ;
#16982 = EDGE_LOOP ( 'NONE', ( #4790, #903, #18100, #13301 ) ) ;
#16983 = CARTESIAN_POINT ( 'NONE',  ( 1.389792438032094735, 52.96007428365597036, 75.46169036918907125 ) ) ;
#16984 = CIRCLE ( 'NONE', #15974, 3.999999999999996447 ) ;
#16985 = VECTOR ( 'NONE', #2360, 1000.000000000000000 ) ;
#16986 = EDGE_LOOP ( 'NONE', ( #8456, #8379, #5074, #21027 ) ) ;
#16987 = CARTESIAN_POINT ( 'NONE',  ( 6.946924939155297629, 50.35687629745329019, 76.28194508213313441 ) ) ;
#16988 = CARTESIAN_POINT ( 'NONE',  ( -1.477846259693495146, 50.16218137147969713, 83.55433879953099563 ) ) ;
#16989 = CARTESIAN_POINT ( 'NONE',  ( -2.416137431568557314, 39.07291177436112406, 95.02371380123797451 ) ) ;
#16990 = B_SPLINE_SURFACE_WITH_KNOTS ( 'NONE', 3, 1, ( 
 ( #2247, #8746 ),
 ( #3727, #8322 ),
 ( #19688, #5112 ),
 ( #10246, #15232 ),
 ( #6816, #19795 ),
 ( #15128, #537 ),
 ( #5423, #11942 ),
 ( #11733, #14901 ),
 ( #7127, #13628 ),
 ( #20104, #16513 ),
 ( #5541, #11631 ) ),
 .UNSPECIFIED., .F., .F., .F.,
 ( 4, 1, 1, 1, 1, 1, 1, 1, 4 ),
 ( 2, 2 ),
 ( 0.000000000000000000, 0.1532941345222613438, 0.2882053437387906425, 0.4087820921566970855, 0.5188196696909340710, 0.6272811593758456095, 0.7389121241215087510, 0.8614321729660930904, 1.000000000000000000 ),
 ( 0.000000000000000000, 1.000000000000000000 ),
 .UNSPECIFIED. ) ;
#16991 = CARTESIAN_POINT ( 'NONE',  ( -3.416741549526295163, 52.16336322705762996, 76.06019729239972094 ) ) ;
#16992 = VERTEX_POINT ( 'NONE', #4277 ) ;
#16993 = EDGE_CURVE ( 'NONE', #13992, #18313, #15049, .T. ) ;
#16994 = AXIS2_PLACEMENT_3D ( 'NONE', #5799, #4200, #4703 ) ;
#16995 = CARTESIAN_POINT ( 'NONE',  ( -0.9436870690626137925, 52.23009998296729606, 72.45433879953087342 ) ) ;
#16996 = VERTEX_POINT ( 'NONE', #5986 ) ;
#16997 = CARTESIAN_POINT ( 'NONE',  ( 4.552551799799910981, 51.21148827903365941, 79.39429067157672648 ) ) ;
#16998 = CARTESIAN_POINT ( 'NONE',  ( 23.63948732994508006, 45.16218137147969003, 76.90433879953101837 ) ) ;
#16999 = CARTESIAN_POINT ( 'NONE',  ( 27.03948732994508930, 43.16218137147969003, 76.90433879953101837 ) ) ;
#17000 = CARTESIAN_POINT ( 'NONE',  ( 4.104125825492272561, 51.53190454079617666, 76.88467537290178200 ) ) ;
#17001 = CARTESIAN_POINT ( 'NONE',  ( 3.357643116058062205, 50.56218137147968861, 92.03489701350649455 ) ) ;
#17002 = CARTESIAN_POINT ( 'NONE',  ( -4.567115856812060670, 47.10047254335474065, 95.96121380123798872 ) ) ;
#17003 = AXIS2_PLACEMENT_3D ( 'NONE', #9277, #10566, #19053 ) ;
#17004 = CARTESIAN_POINT ( 'NONE',  ( 8.790110392356673685, 41.13824298228534104, 76.23356602378127889 ) ) ;
#17005 = CARTESIAN_POINT ( 'NONE',  ( 31.07218010054375412, 45.56218137147968861, 70.80574467885102763 ) ) ;
#17006 = CARTESIAN_POINT ( 'NONE',  ( -4.677846259693496656, 44.16218127507082158, 94.26911326394257173 ) ) ;
#17007 = CARTESIAN_POINT ( 'NONE',  ( -0.8237052942265477018, 49.18499566818285018, 91.50808880294498238 ) ) ;
#17008 = AXIS2_PLACEMENT_3D ( 'NONE', #18039, #13458, #8465 ) ;
#17009 = EDGE_CURVE ( 'NONE', #5038, #1468, #10708, .T. ) ;
#17010 = DIRECTION ( 'NONE',  ( -0.000000000000000000, -0.000000000000000000, 1.000000000000000000 ) ) ;
#17011 = EDGE_LOOP ( 'NONE', ( #6484, #17188, #5254, #18777 ) ) ;
#17012 = CARTESIAN_POINT ( 'NONE',  ( 8.348147950866749767, 41.73372909538741027, 78.88894238123772595 ) ) ;
#17013 = ORIENTED_EDGE ( 'NONE', *, *, #13676, .T. ) ;
#17014 = DIRECTION ( 'NONE',  ( 1.000000000000000000, 0.000000000000000000, 0.000000000000000000 ) ) ;
#17015 = DIRECTION ( 'NONE',  ( -1.000000000000000000, 1.193617070626243484E-16, 0.000000000000000000 ) ) ;
#17016 = CARTESIAN_POINT ( 'NONE',  ( -3.448881463449838591, 52.14039722128521959, 78.93778436892569061 ) ) ;
#17017 = CARTESIAN_POINT ( 'NONE',  ( 5.611423337425062385, 41.22389019960463230, 92.83621380123797451 ) ) ;
#17018 = CARTESIAN_POINT ( 'NONE',  ( -4.518657848439217695, 36.94521123081658942, 76.91875223014945107 ) ) ;
#17019 = DIRECTION ( 'NONE',  ( -1.000000000000000000, -1.402518428993831676E-16, -1.196361017915039239E-16 ) ) ;
#17020 = DIRECTION ( 'NONE',  ( -0.5941461771852041274, -0.8043570849667502909, 3.170109439321510848E-15 ) ) ;
#17021 = EDGE_CURVE ( 'NONE', #20176, #14506, #1207, .T. ) ;
#17022 = CARTESIAN_POINT ( 'NONE',  ( 11.22215374030650281, 42.96218137147968008, 61.80715055817104542 ) ) ;
#17023 = ORIENTED_EDGE ( 'NONE', *, *, #13038, .F. ) ;
#17024 = ORIENTED_EDGE ( 'NONE', *, *, #2413, .F. ) ;
#17025 = EDGE_CURVE ( 'NONE', #1059, #5621, #9330, .T. ) ;
#17026 = UNCERTAINTY_MEASURE_WITH_UNIT (LENGTH_MEASURE( 1.000000000000000082E-05 ), #13373, 'distance_accuracy_value', 'NONE');
#17027 = CARTESIAN_POINT ( 'NONE',  ( 6.461593583102923866, 49.81579045121515747, 77.32164228125272132 ) ) ;
#17028 = FACE_OUTER_BOUND ( 'NONE', #17776, .T. ) ;
#17029 = CARTESIAN_POINT ( 'NONE',  ( 1.514255888186008425, 52.36218137147968577, 48.36106904222365444 ) ) ;
#17030 = CARTESIAN_POINT ( 'NONE',  ( 24.32215374030650068, 44.16218137147968292, 93.55433879953098142 ) ) ;
#17031 = CARTESIAN_POINT ( 'NONE',  ( 0.5221537403065181771, 44.16218137147969003, 56.15433879953099705 ) ) ;
#17032 = CARTESIAN_POINT ( 'NONE',  ( 8.344156084401983975, 42.16610768104432339, 78.13567616980381558 ) ) ;
#17033 = CARTESIAN_POINT ( 'NONE',  ( 1.868012774839550749, 39.13936707477651566, 92.13308880294498238 ) ) ;
#17034 = ADVANCED_FACE ( 'NONE', ( #9201 ), #9403, .T. ) ;
#17035 = CIRCLE ( 'NONE', #381, 6.199999999999999289 ) ;
#17036 = EDGE_CURVE ( 'NONE', #19846, #15434, #14779, .T. ) ;
#17037 = CARTESIAN_POINT ( 'NONE',  ( -4.388425821632080392, 51.46903322184264340, 76.24813767079230331 ) ) ;
#17038 = EDGE_CURVE ( 'NONE', #15353, #14869, #6601, .T. ) ;
#17039 = CARTESIAN_POINT ( 'NONE',  ( -7.726407013549337677, 47.24009745779464708, 77.87251963618699335 ) ) ;
#17040 = CARTESIAN_POINT ( 'NONE',  ( -4.567115856812060670, 47.10047254335474065, 92.05496380123798872 ) ) ;
#17041 = B_SPLINE_SURFACE_WITH_KNOTS ( 'NONE', 3, 1, ( 
 ( #14776, #12025 ),
 ( #3600, #8296 ),
 ( #3810, #10329 ),
 ( #8620, #197 ),
 ( #19869, #3698 ),
 ( #19661, #1906 ),
 ( #5088, #18081 ),
 ( #10009, #8398 ),
 ( #5290, #16801 ),
 ( #15101, #14877 ),
 ( #6988, #6791 ),
 ( #13297, #19768 ),
 ( #5190, #15315 ),
 ( #12437, #20401 ),
 ( #9037, #20287 ),
 ( #5832, #727 ),
 ( #15523, #16900 ),
 ( #1160, #8818 ),
 ( #938, #17327 ),
 ( #7425, #13810 ),
 ( #18916, #5719 ),
 ( #4228, #12337 ),
 ( #4331, #4121 ),
 ( #13919, #2322 ),
 ( #19024, #10436 ),
 ( #1053, #7210 ),
 ( #13711, #20186 ) ),
 .UNSPECIFIED., .F., .F., .F.,
 ( 4, 1, 1, 1, 1, 1, 1, 1, 1, 1, 1, 1, 1, 1, 1, 1, 1, 1, 1, 1, 1, 1, 1, 1, 4 ),
 ( 2, 2 ),
 ( 0.000000000000000000, 0.05111620615384394190, 0.09904209687041264087, 0.1432334450931441461, 0.1843589373079111415, 0.2222937343119009146, 0.2574440974212286459, 0.2893637488079585096, 0.3188910630028964910, 0.3474602836591745292, 0.3767670824238625316, 0.4074295047838343287, 0.4392621747742110894, 0.4730325979957886173, 0.5084852716492808122, 0.5462542205972961140, 0.5860610780164621225, 0.6283505634423164343, 0.6729648726644925638, 0.7201947540188263774, 0.7701882088044430530, 0.8230700400259792771, 0.8789456997408242600, 0.9378877171948971636, 1.000000000000000000 ),
 ( 0.000000000000000000, 1.000000000000000000 ),
 .UNSPECIFIED. ) ;
#17042 = DIRECTION ( 'NONE',  ( 1.000000000000000000, -0.000000000000000000, -0.000000000000000000 ) ) ;
#17043 = CARTESIAN_POINT ( 'NONE',  ( 0.5221537403065019678, 51.36218137147968577, 52.53721119516358584 ) ) ;
#17044 = EDGE_CURVE ( 'NONE', #19613, #14176, #7619, .T. ) ;
#17045 = CARTESIAN_POINT ( 'NONE',  ( 5.908589799165438805, 51.12385263867304275, 77.19464465032660883 ) ) ;
#17046 = VERTEX_POINT ( 'NONE', #19481 ) ;
#17047 = AXIS2_PLACEMENT_3D ( 'NONE', #14056, #15775, #1187 ) ;
#17048 = DIRECTION ( 'NONE',  ( -1.000000000000000000, 0.000000000000000000, -0.000000000000000000 ) ) ;
#17049 = AXIS2_PLACEMENT_3D ( 'NONE', #1169, #14133, #4647 ) ;
#17050 = CARTESIAN_POINT ( 'NONE',  ( 3.460444912181559474, 49.25145096859824889, 91.74246380123798872 ) ) ;
#17051 = ORIENTED_EDGE ( 'NONE', *, *, #7806, .T. ) ;
#17052 = CARTESIAN_POINT ( 'NONE',  ( 2.921181103050038086, 49.30691215337508737, 94.75121379782399345 ) ) ;
#17053 = DIRECTION ( 'NONE',  ( 1.402518428993831676E-16, -1.000000000000000000, 1.677918375355662166E-32 ) ) ;
#17054 = CARTESIAN_POINT ( 'NONE',  ( -3.657653629913878657, 51.07144069248850116, 79.48422614141084352 ) ) ;
#17055 = DIRECTION ( 'NONE',  ( -1.000000000000000000, -1.402518428993831676E-16, -1.196361017915039239E-16 ) ) ;
#17056 = CARTESIAN_POINT ( 'NONE',  ( 0.4173134239696620895, 52.36160896100310680, 77.42739361215659244 ) ) ;
#17057 = CARTESIAN_POINT ( 'NONE',  ( -3.361985906478571984, 37.00483926610629482, 79.26586447293077242 ) ) ;
#17058 = ORIENTED_EDGE ( 'NONE', *, *, #4824, .T. ) ;
#17059 = DIRECTION ( 'NONE',  ( 1.540237394707284220E-16, 1.793354297423764243E-16, -1.000000000000000000 ) ) ;
#17060 = ORIENTED_EDGE ( 'NONE', *, *, #9049, .T. ) ;
#17061 = CARTESIAN_POINT ( 'NONE',  ( 6.389146928619912735, 49.89105453160614445, 77.93146757323737006 ) ) ;
#17062 = CARTESIAN_POINT ( 'NONE',  ( 4.584522445964598347, 52.10188785579612158, 77.22170381446332499 ) ) ;
#17063 = DIRECTION ( 'NONE',  ( -1.540237394707284220E-16, -1.793354297423764243E-16, 1.000000000000000000 ) ) ;
#17064 = CARTESIAN_POINT ( 'NONE',  ( 31.07218010054375412, 42.76218137147968434, 70.80574467885102763 ) ) ;
#17065 = CARTESIAN_POINT ( 'NONE',  ( -1.477846259693489372, 49.81903562097208038, 53.15433879953100416 ) ) ;
#17066 = CARTESIAN_POINT ( 'NONE',  ( 2.263363662449358493, 49.77488197367694767, 94.36419268333823140 ) ) ;
#17067 = AXIS2_PLACEMENT_3D ( 'NONE', #12791, #15994, #1208 ) ;
#17068 = CARTESIAN_POINT ( 'NONE',  ( 4.673174852049361228, 39.63213674411673537, 94.36058879782399345 ) ) ;
#17069 = EDGE_CURVE ( 'NONE', #11136, #7228, #6288, .T. ) ;
#17070 = CARTESIAN_POINT ( 'NONE',  ( -5.561099455747291032, 37.71522085402570212, 75.56266266290518274 ) ) ;
#17071 = AXIS2_PLACEMENT_3D ( 'NONE', #13852, #5770, #17260 ) ;
#17072 = ORIENTED_EDGE ( 'NONE', *, *, #863, .F. ) ;
#17073 = EDGE_CURVE ( 'NONE', #16819, #4837, #20958, .T. ) ;
#17074 = CARTESIAN_POINT ( 'NONE',  ( 4.183728870144529211, 51.49929324773223271, 77.32903872825052360 ) ) ;
#17075 = ORIENTED_EDGE ( 'NONE', *, *, #2865, .F. ) ;
#17076 = CARTESIAN_POINT ( 'NONE',  ( 8.865792162213244509, 41.36506604770743678, 78.93669174070734584 ) ) ;
#17077 = CARTESIAN_POINT ( 'NONE',  ( -0.8237052942265477018, 49.18499566818285018, 92.44558879953099506 ) ) ;
#17078 = ORIENTED_EDGE ( 'NONE', *, *, #9388, .F. ) ;
#17079 = CARTESIAN_POINT ( 'NONE',  ( 2.043125170982144745, 38.48583871533720213, 95.17996380123798872 ) ) ;
#17080 = CARTESIAN_POINT ( 'NONE',  ( 2.492135536370527316, 38.60615068013622420, 95.03863327408673456 ) ) ;
#17081 = ORIENTED_EDGE ( 'NONE', *, *, #1943, .F. ) ;
#17082 = VECTOR ( 'NONE', #19105, 1000.000000000000000 ) ;
#17083 = CARTESIAN_POINT ( 'NONE',  ( 4.199109002476567376, 47.83913663364971569, 83.28180655319408743 ) ) ;
#17084 = DIRECTION ( 'NONE',  ( 3.893792155548169402E-16, 7.183611964723547524E-17, -1.000000000000000000 ) ) ;
#17085 = EDGE_CURVE ( 'NONE', #8173, #6536, #10355, .T. ) ;
#17086 = VECTOR ( 'NONE', #3906, 1000.000000000000000 ) ;
#17087 = EDGE_LOOP ( 'NONE', ( #19370, #12244, #5685, #16475 ) ) ;
#17088 = CARTESIAN_POINT ( 'NONE',  ( 11.22215374030650281, 42.96218137147968008, 73.80433879953100984 ) ) ;
#17089 = CARTESIAN_POINT ( 'NONE',  ( 5.568489401881125289, 48.03437091500646261, 95.57058880123798872 ) ) ;
#17090 = ORIENTED_EDGE ( 'NONE', *, *, #13273, .T. ) ;
#17091 = CARTESIAN_POINT ( 'NONE',  ( -4.863118049607145110, 50.34667215411423058, 79.41941354504645290 ) ) ;
#17092 = CARTESIAN_POINT ( 'NONE',  ( 0.5221537403065015237, 44.16218137147968292, 75.45433879953087342 ) ) ;
#17093 = B_SPLINE_CURVE_WITH_KNOTS ( 'NONE', 3,
 ( #10502, #20148, #16967, #20248, #6955, #3771, #12083, #8899, #5360, #4196, #12301, #13775, #10722, #3875, #20041, #17182, #16766, #10290, #578, #2605, #18459, #5677, #4086, #8684 ),
 .UNSPECIFIED., .F., .F.,
 ( 4, 2, 2, 2, 2, 2, 2, 2, 2, 2, 2, 4 ),
 ( 0.000000000000000000, 0.001310659670290844356, 0.001965989505436258403, 0.002621319340581672232, 0.003931979010872510734, 0.005242638681163349669, 0.006553298351454187737, 0.007208628186599608072, 0.007863958021745026672, 0.008519287856890446139, 0.009174617692035867342, 0.01048527736232670628 ),
 .UNSPECIFIED. ) ;
#17094 = PRODUCT_CONTEXT ( 'NONE', #2614, 'mechanical' ) ;
#17095 = CARTESIAN_POINT ( 'NONE',  ( -4.718161399584267279, 37.09257646755418847, 75.97198585835440099 ) ) ;
#17096 = CARTESIAN_POINT ( 'NONE',  ( 5.239313537742215310, 50.86510457629285042, 78.59183879953087626 ) ) ;
#17097 = CIRCLE ( 'NONE', #18781, 8.199999999999995737 ) ;
#17098 = FACE_OUTER_BOUND ( 'NONE', #456, .T. ) ;
#17099 = ORIENTED_EDGE ( 'NONE', *, *, #10957, .T. ) ;
#17100 = CARTESIAN_POINT ( 'NONE',  ( -1.123656915330052408, 35.37488560990637865, 76.86610350541323555 ) ) ;
#17101 = ORIENTED_EDGE ( 'NONE', *, *, #12510, .F. ) ;
#17102 = CARTESIAN_POINT ( 'NONE',  ( 6.961907239250668233, 50.34580947589670075, 76.63889762306028786 ) ) ;
#17103 = LINE ( 'NONE', #16988, #4124 ) ;
#17104 = CARTESIAN_POINT ( 'NONE',  ( 6.828503391016846891, 43.33193468930419101, 95.25808880123800293 ) ) ;
#17105 = ORIENTED_EDGE ( 'NONE', *, *, #3619, .T. ) ;
#17106 = CARTESIAN_POINT ( 'NONE',  ( 6.266852414816192152, 50.85921847619028568, 79.48482414599367019 ) ) ;
#17107 = ORIENTED_EDGE ( 'NONE', *, *, #14354, .F. ) ;
#17108 = CARTESIAN_POINT ( 'NONE',  ( 5.760694563098077481, 51.23309689197250094, 79.54845644658969661 ) ) ;
#17109 = CARTESIAN_POINT ( 'NONE',  ( -1.477846259693491593, 47.62628298661744708, 53.15433879953100416 ) ) ;
#17110 = CARTESIAN_POINT ( 'NONE',  ( 7.671391872361274622, 40.16655736720171888, 76.83374382764255017 ) ) ;
#17111 = VECTOR ( 'NONE', #10001, 1000.000000000000114 ) ;
#17112 = CARTESIAN_POINT ( 'NONE',  ( -4.917446439638588629, 37.23978029895123143, 77.90454030471208569 ) ) ;
#17113 = CARTESIAN_POINT ( 'NONE',  ( 4.539621438837683876, 52.13505442103787857, 76.64209438045911327 ) ) ;
#17114 = CARTESIAN_POINT ( 'NONE',  ( -7.600977292165548072, 43.04172748006588023, 78.91532537708295081 ) ) ;
#17115 = PLANE ( 'NONE',  #14394 ) ;
#17116 = DIRECTION ( 'NONE',  ( 0.000000000000000000, 1.000000000000000000, 0.000000000000000000 ) ) ;
#17117 = DIRECTION ( 'NONE',  ( -0.000000000000000000, -2.168404344970984413E-15, -1.000000000000000000 ) ) ;
#17118 = CARTESIAN_POINT ( 'NONE',  ( 5.025485839985549319, 41.56218137147963887, 91.03933880294498238 ) ) ;
#17119 = ORIENTED_EDGE ( 'NONE', *, *, #16023, .F. ) ;
#17120 = CARTESIAN_POINT ( 'NONE',  ( 8.871704507997348443, 41.38278572309461367, 78.93627637315103129 ) ) ;
#17121 = VECTOR ( 'NONE', #17544, 1000.000000000000227 ) ;
#17122 = VERTEX_POINT ( 'NONE', #7900 ) ;
#17123 = CARTESIAN_POINT ( 'NONE',  ( -7.677846259693480668, 44.16218137147969003, 54.55433879953099563 ) ) ;
#17124 = CARTESIAN_POINT ( 'NONE',  ( -6.254105203661088908, 41.71089193230473313, 78.61536821129558916 ) ) ;
#17125 = CARTESIAN_POINT ( 'NONE',  ( -4.092737432821778931, 51.68032131864361389, 79.48422614141084352 ) ) ;
#17126 = CARTESIAN_POINT ( 'NONE',  ( -1.077846259693492126, 49.76218137147969856, 53.55433879953100273 ) ) ;
#17127 = CARTESIAN_POINT ( 'NONE',  ( -4.641234702847270910, 37.03575381547093315, 77.24798498253255730 ) ) ;
#17128 = CARTESIAN_POINT ( 'NONE',  ( -7.883865680119443553, 46.78753189708820770, 79.41298732254628590 ) ) ;
#17129 = CARTESIAN_POINT ( 'NONE',  ( 5.435172323252741577, 36.85707235623052469, 77.60331851759366373 ) ) ;
#17130 = EDGE_CURVE ( 'NONE', #3704, #7517, #3311, .T. ) ;
#17131 = CARTESIAN_POINT ( 'NONE',  ( -4.357516591192299060, 37.58081861725695205, 75.97198585835440099 ) ) ;
#17132 = ORIENTED_EDGE ( 'NONE', *, *, #14052, .F. ) ;
#17133 = EDGE_LOOP ( 'NONE', ( #8551, #17300, #19396, #7120 ) ) ;
#17134 = DIRECTION ( 'NONE',  ( -0.9480563259966822143, -0.3181025035073955509, -2.030702297275135124E-16 ) ) ;
#17135 = CARTESIAN_POINT ( 'NONE',  ( -4.412760631825748625, 36.86698922270430501, 75.37821288891845484 ) ) ;
#17136 = DIRECTION ( 'NONE',  ( -1.000000000000000000, -1.402518428993831676E-16, -1.196361017915039239E-16 ) ) ;
#17137 = LINE ( 'NONE', #13623, #7932 ) ;
#17138 = CARTESIAN_POINT ( 'NONE',  ( 8.921473627994183531, 41.53194693301924190, 77.48121952543638713 ) ) ;
#17139 = LINE ( 'NONE', #4040, #7831 ) ;
#17140 = CARTESIAN_POINT ( 'NONE',  ( -0.2125050281363792815, 38.58189400963055959, 92.05496380294498238 ) ) ;
#17141 = DIRECTION ( 'NONE',  ( -0.6080936526121289987, -0.7938652969193448206, -2.360290325043240801E-16 ) ) ;
#17142 = EDGE_CURVE ( 'NONE', #17381, #8776, #20277, .T. ) ;
#17143 = CARTESIAN_POINT ( 'NONE',  ( -7.686167599515409066, 47.36069753439516461, 78.25347377718505015 ) ) ;
#17144 = CARTESIAN_POINT ( 'NONE',  ( -5.507474035114395150, 38.61161641206103212, 78.58503192925951453 ) ) ;
#17145 = CARTESIAN_POINT ( 'NONE',  ( -8.106954325919813797, 42.43031530731593648, 79.37810177255154542 ) ) ;
#17146 = VERTEX_POINT ( 'NONE', #19272 ) ;
#17147 = LINE ( 'NONE', #10782, #19081 ) ;
#17148 = ADVANCED_FACE ( 'NONE', ( #16416 ), #9932, .F. ) ;
#17149 = ORIENTED_EDGE ( 'NONE', *, *, #2497, .T. ) ;
#17150 = CARTESIAN_POINT ( 'NONE',  ( -4.618682869335207108, 51.30449996580257022, 78.93596273702843291 ) ) ;
#17151 = CARTESIAN_POINT ( 'NONE',  ( -3.981178359372548492, 46.76218137147973408, 91.66433880294496817 ) ) ;
#17152 = ORIENTED_EDGE ( 'NONE', *, *, #16424, .F. ) ;
#17153 = EDGE_CURVE ( 'NONE', #9281, #3928, #12896, .T. ) ;
#17154 = CARTESIAN_POINT ( 'NONE',  ( 32.52215374030650707, 44.16218137147969003, 105.5543387995309956 ) ) ;
#17155 = CARTESIAN_POINT ( 'NONE',  ( -0.7151367401353951880, 52.21770371292401336, 75.80943630940421940 ) ) ;
#17156 = CARTESIAN_POINT ( 'NONE',  ( -3.653812822066824673, 51.99396077543343608, 79.24282704039583791 ) ) ;
#17157 = CARTESIAN_POINT ( 'NONE',  ( 6.691294758883309157, 37.75465145915448062, 79.45433879953087342 ) ) ;
#17158 = CARTESIAN_POINT ( 'NONE',  ( 5.394726803408538274, 50.74878659197170805, 77.28963291717792572 ) ) ;
#17159 = CARTESIAN_POINT ( 'NONE',  ( -3.533668833548941013, 36.21763952329489200, 78.50831005042292077 ) ) ;
#17160 = EDGE_LOOP ( 'NONE', ( #5884, #2958, #7789, #15448 ) ) ;
#17161 = FACE_BOUND ( 'NONE', #13074, .T. ) ;
#17162 = ORIENTED_EDGE ( 'NONE', *, *, #8291, .F. ) ;
#17163 = DIRECTION ( 'NONE',  ( 1.000000000000000000, -1.193617070626243484E-16, 0.000000000000000000 ) ) ;
#17164 = DIRECTION ( 'NONE',  ( 0.3165065846431828200, 0.9485903129789527988, 0.000000000000000000 ) ) ;
#17165 = ADVANCED_FACE ( 'NONE', ( #17684 ), #16096, .F. ) ;
#17166 = LINE ( 'NONE', #3065, #18338 ) ;
#17167 = CARTESIAN_POINT ( 'NONE',  ( 0.6452163281857689059, 52.96132085210302165, 79.54845644658969661 ) ) ;
#17168 = CARTESIAN_POINT ( 'NONE',  ( 31.07218010054375412, 45.56218137147968861, 64.80574467885102763 ) ) ;
#17169 = DIRECTION ( 'NONE',  ( 0.7071067811865460184, 9.917302918806395333E-17, 0.7071067811865490160 ) ) ;
#17170 = CARTESIAN_POINT ( 'NONE',  ( 5.081221074959174189, 37.34619514398751505, 78.14228948390012874 ) ) ;
#17171 = ORIENTED_EDGE ( 'NONE', *, *, #4599, .F. ) ;
#17172 = CARTESIAN_POINT ( 'NONE',  ( -0.02399531697664270338, 35.98038931794833672, 79.45433879953087342 ) ) ;
#17173 = VERTEX_POINT ( 'NONE', #6392 ) ;
#17174 = DIRECTION ( 'NONE',  ( 1.000000000000000000, -0.000000000000000000, -0.000000000000000000 ) ) ;
#17175 = CARTESIAN_POINT ( 'NONE',  ( -5.058133621542618030, 44.89684013992257405, 96.42996379953098085 ) ) ;
#17176 = CARTESIAN_POINT ( 'NONE',  ( -7.228585422969530327, 41.91720008378919005, 77.67112630499640602 ) ) ;
#17177 = EDGE_LOOP ( 'NONE', ( #7598, #15727, #14458, #18347 ) ) ;
#17178 = EDGE_CURVE ( 'NONE', #3682, #13937, #17790, .T. ) ;
#17179 = CARTESIAN_POINT ( 'NONE',  ( 5.568489401881125289, 48.03437091500646261, 91.82058880123797451 ) ) ;
#17180 = CARTESIAN_POINT ( 'NONE',  ( -1.419351766502868761, 49.49642391118513274, 94.75121379782397923 ) ) ;
#17181 = CARTESIAN_POINT ( 'NONE',  ( 0.5221537403065019678, 44.16218137147968292, 72.45433879953087342 ) ) ;
#17182 = CARTESIAN_POINT ( 'NONE',  ( 1.018894512563303545, 38.97592790927090789, 95.05433879953099563 ) ) ;
#17183 = CARTESIAN_POINT ( 'NONE',  ( -4.655845291449849377, 51.27794505956256188, 78.93463708245236887 ) ) ;
#17184 = ADVANCED_FACE ( 'NONE', ( #19581 ), #6643, .F. ) ;
#17185 = ORIENTED_EDGE ( 'NONE', *, *, #10036, .T. ) ;
#17186 = CARTESIAN_POINT ( 'NONE',  ( 0.5221537403065181771, 44.16218137147969003, 56.15433879953099705 ) ) ;
#17187 = CARTESIAN_POINT ( 'NONE',  ( 0.7836272451433452524, 52.96402169819676686, 78.85266037376247539 ) ) ;
#17188 = ORIENTED_EDGE ( 'NONE', *, *, #17818, .T. ) ;
#17189 = CARTESIAN_POINT ( 'NONE',  ( -5.395957697070454806, 49.83809498072223931, 78.51765637652050600 ) ) ;
#17190 = DIRECTION ( 'NONE',  ( 1.000000000000000000, -0.000000000000000000, -0.000000000000000000 ) ) ;
#17191 = EDGE_CURVE ( 'NONE', #18638, #14937, #6535, .T. ) ;
#17192 =( BOUNDED_SURFACE ( )  B_SPLINE_SURFACE ( 1, 2, ( 
 ( #9034, #13490, #15198, #15520, #17002, #6984, #19962, #13915, #10326, #20398, #2431, #5829, #724, #13708, #7318, #20074, #5391, #18815, #2319, #10431, #12022, #18496, #16897, #11910, #8815, #20183, #18385, #5613, #8928, #15417, #9456, #4543, #11158, #7745, #14227, #6341, #2951, #1472, #19021, #20815, #7956, #16050, #12435, #9356, #12746, #15841, #17627, #15738, #1050, #3171, #19323, #14439, #11057, #7535, #11268, #20910, #12646, #1158, #20705, #17324, #15628, #17530, #14341, #15942, #14024, #12845, #17739, #4328, #4739, #20606, #20507, #10955, #6243, #7643, #14124, #1253, #1364, #3060, #7855, #5938, #6144 ),
 ( #9252, #19128, #19222, #4639, #10856, #9567, #2747, #4442, #6034, #12535, #17428, #2853, #14961, #17842, #176, #9674, #13163, #9985, #16464, #16360, #1790, #11681, #10081, #6446, #9769, #1677, #6556, #13063, #4954, #1885, #17945, #3366, #9877, #8271, #14755, #5747, #4741, #14548, #4150, #5860, #1575, #4248, #1182, #17239, #6342, #7565, #21013, #6447, #538, #5217, #8852, #4119, #14027, #10434, #7207, #7068, #9114, #703, #3987, #18362, #15396, #2193, #15602, #7183, #2295, #8691, #20050, #10299, #20257, #5483, #11998, #7511, #18468, #3885, #10407, #16875, #13684, #5368, #20160, #1018, #9012 ) ),
 .UNSPECIFIED., .F., .F., .F. ) 
 B_SPLINE_SURFACE_WITH_KNOTS ( ( 2, 2 ),
 ( 3, 2, 2, 2, 2, 2, 2, 2, 2, 2, 2, 2, 2, 2, 2, 2, 2, 2, 2, 2, 2, 2, 2, 2, 2, 2, 2, 2, 2, 2, 2, 2, 2, 2, 2, 2, 2, 2, 2, 2, 3 ),
 ( 0.000000000000000000, 1.000000000000000000 ),
 ( 0.000000000000000000, 0.02500000000000000139, 0.05000000000000000278, 0.07499999999999999722, 0.1000000000000000056, 0.1250000000000000000, 0.1499999999999999944, 0.1749999999999999889, 0.2000000000000000111, 0.2250000000000000056, 0.2500000000000000000, 0.2750000000000000222, 0.2999999999999999889, 0.3250000000000000111, 0.3499999999999999778, 0.3750000000000000000, 0.4000000000000000222, 0.4249999999999999889, 0.4500000000000000111, 0.4749999999999999778, 0.5000000000000000000, 0.5250000000000000222, 0.5500000000000000444, 0.5749999999999999556, 0.5999999999999999778, 0.6250000000000000000, 0.6500000000000000222, 0.6750000000000000444, 0.6999999999999999556, 0.7249999999999999778, 0.7500000000000000000, 0.7750000000000000222, 0.8000000000000000444, 0.8249999999999999556, 0.8499999999999999778, 0.8750000000000000000, 0.9000000000000000222, 0.9250000000000000444, 0.9499999999999999556, 0.9600309411673831894, 0.9696312505790569691 ),
 .UNSPECIFIED. ) 
 GEOMETRIC_REPRESENTATION_ITEM ( )  RATIONAL_B_SPLINE_SURFACE ( (
 ( 1.000000000000000000, 0.9238795325112867385, 1.000000000000000000, 0.9238795325112867385, 1.000000000000000000, 0.9238795325112867385, 1.000000000000000000, 0.9238795325112867385, 1.000000000000000000, 0.9238795325112867385, 1.000000000000000000, 0.9238795325112867385, 1.000000000000000000, 0.9238795325112867385, 1.000000000000000000, 0.9238795325112867385, 1.000000000000000000, 0.9238795325112867385, 1.000000000000000000, 0.9238795325112867385, 1.000000000000000000, 0.9238795325112867385, 1.000000000000000000, 0.9238795325112867385, 1.000000000000000000, 0.9238795325112867385, 1.000000000000000000, 0.9238795325112867385, 1.000000000000000000, 0.9238795325112867385, 1.000000000000000000, 0.9238795325112867385, 1.000000000000000000, 0.9238795325112867385, 1.000000000000000000, 0.9238795325112867385, 1.000000000000000000, 0.9238795325112867385, 1.000000000000000000, 0.9238795325112867385, 1.000000000000000000, 0.9238795325112867385, 1.000000000000000000, 0.9238795325112867385, 1.000000000000000000, 0.9238795325112867385, 1.000000000000000000, 0.9238795325112867385, 1.000000000000000000, 0.9238795325112867385, 1.000000000000000000, 0.9238795325112867385, 1.000000000000000000, 0.9238795325112867385, 1.000000000000000000, 0.9238795325112867385, 1.000000000000000000, 0.9238795325112867385, 1.000000000000000000, 0.9238795325112867385, 1.000000000000000000, 0.9238795325112867385, 1.000000000000000000, 0.9238795325112867385, 1.000000000000000000, 0.9238795325112867385, 1.000000000000000000, 0.9238795325112867385, 1.000000000000000000, 0.9238795325112867385, 1.000000000000000000, 0.9238795325112867385, 1.000000000000000000, 0.9238795325112867385, 1.000000000000000000, 0.9238795325112867385, 1.000000000000000000, 0.9694576027594803413, 0.9634247247054007479, 0.9634247247054007479, 0.9634247247054007479),
 ( 1.000000000000000000, 0.9238795325112867385, 1.000000000000000000, 0.9238795325112867385, 1.000000000000000000, 0.9238795325112867385, 1.000000000000000000, 0.9238795325112867385, 1.000000000000000000, 0.9238795325112867385, 1.000000000000000000, 0.9238795325112867385, 1.000000000000000000, 0.9238795325112867385, 1.000000000000000000, 0.9238795325112867385, 1.000000000000000000, 0.9238795325112867385, 1.000000000000000000, 0.9238795325112867385, 1.000000000000000000, 0.9238795325112867385, 1.000000000000000000, 0.9238795325112867385, 1.000000000000000000, 0.9238795325112867385, 1.000000000000000000, 0.9238795325112867385, 1.000000000000000000, 0.9238795325112867385, 1.000000000000000000, 0.9238795325112867385, 1.000000000000000000, 0.9238795325112867385, 1.000000000000000000, 0.9238795325112867385, 1.000000000000000000, 0.9238795325112867385, 1.000000000000000000, 0.9238795325112867385, 1.000000000000000000, 0.9238795325112867385, 1.000000000000000000, 0.9238795325112867385, 1.000000000000000000, 0.9238795325112867385, 1.000000000000000000, 0.9238795325112867385, 1.000000000000000000, 0.9238795325112867385, 1.000000000000000000, 0.9238795325112867385, 1.000000000000000000, 0.9238795325112867385, 1.000000000000000000, 0.9238795325112867385, 1.000000000000000000, 0.9238795325112867385, 1.000000000000000000, 0.9238795325112867385, 1.000000000000000000, 0.9238795325112867385, 1.000000000000000000, 0.9238795325112867385, 1.000000000000000000, 0.9238795325112867385, 1.000000000000000000, 0.9238795325112867385, 1.000000000000000000, 0.9238795325112867385, 1.000000000000000000, 0.9238795325112867385, 1.000000000000000000, 0.9238795325112867385, 1.000000000000000000, 0.9238795325112867385, 1.000000000000000000, 0.9694576027594803413, 0.9634247247054007479, 0.9634247247054007479, 0.9634247247054007479) ) ) 
 REPRESENTATION_ITEM ( '' )  SURFACE ( )  );
#17193 = EDGE_CURVE ( 'NONE', #20326, #791, #13059, .T. ) ;
#17194 = SHAPE_DEFINITION_REPRESENTATION ( #3942, #11365 ) ;
#17195 = CARTESIAN_POINT ( 'NONE',  ( -3.955205046931956403, 36.52901134360649138, 77.68963291717793140 ) ) ;
#17196 = CARTESIAN_POINT ( 'NONE',  ( 5.239545088994572275, 50.86493353871018286, 78.62371398036725623 ) ) ;
#17197 = CARTESIAN_POINT ( 'NONE',  ( 0.5221537403065064087, 48.16218137147969003, 58.55433879953100984 ) ) ;
#17198 = ORIENTED_EDGE ( 'NONE', *, *, #11818, .T. ) ;
#17199 = CARTESIAN_POINT ( 'NONE',  ( 1.773874092659751600, 52.95704565865690228, 75.65494847458032268 ) ) ;
#17200 = ORIENTED_EDGE ( 'NONE', *, *, #4257, .T. ) ;
#17201 = CARTESIAN_POINT ( 'NONE',  ( 6.323093812904748923, 50.81767522096397727, 75.43719735689487038 ) ) ;
#17202 = CARTESIAN_POINT ( 'NONE',  ( 4.199109002476567376, 47.83913663364971569, 95.05433879953098142 ) ) ;
#17203 = CARTESIAN_POINT ( 'NONE',  ( -4.524181921268124462, 40.28999182795290324, 91.19558880123797451 ) ) ;
#17204 = ORIENTED_EDGE ( 'NONE', *, *, #18296, .F. ) ;
#17205 = CARTESIAN_POINT ( 'NONE',  ( -3.781340262490589410, 47.93810351720699003, 92.45433879953095868 ) ) ;
#17206 = ORIENTED_EDGE ( 'NONE', *, *, #3758, .T. ) ;
#17207 = PLANE ( 'NONE',  #19947 ) ;
#17208 = CARTESIAN_POINT ( 'NONE',  ( -1.376885767552595174, 38.47063949360596524, 80.45433879953087342 ) ) ;
#17209 = CARTESIAN_POINT ( 'NONE',  ( 7.675929975837751051, 40.18015835121261858, 76.38443001783366526 ) ) ;
#17210 = VECTOR ( 'NONE', #19164, 1000.000000000000000 ) ;
#17211 = ORIENTED_EDGE ( 'NONE', *, *, #219, .T. ) ;
#17212 = CARTESIAN_POINT ( 'NONE',  ( 5.282950423531485917, 37.48574407745871895, 77.76022115247205591 ) ) ;
#17213 = CARTESIAN_POINT ( 'NONE',  ( -7.419930862061532295, 40.07230896987099555, 78.54487611535471103 ) ) ;
#17214 = CARTESIAN_POINT ( 'NONE',  ( 1.652727357819363974, 35.35299279957455099, 79.45433879953087342 ) ) ;
#17215 = EDGE_CURVE ( 'NONE', #16470, #11222, #12376, .T. ) ;
#17216 = CYLINDRICAL_SURFACE ( 'NONE', #812, 4.200000000000003730 ) ;
#17217 = DIRECTION ( 'NONE',  ( -1.402518428993831183E-16, 1.000000000000000000, -3.469446951953617640E-16 ) ) ;
#17218 = CARTESIAN_POINT ( 'NONE',  ( 0.8498507653315134913, 52.95607782800728813, 78.57205668465995529 ) ) ;
#17219 = CARTESIAN_POINT ( 'NONE',  ( -4.500660556396669065, 42.81632233694663370, 94.32058880294496817 ) ) ;
#17220 = CARTESIAN_POINT ( 'NONE',  ( -4.500660556396669065, 42.81632233694663370, 90.57058880294496817 ) ) ;
#17221 = PLANE ( 'NONE',  #6190 ) ;
#17222 = VECTOR ( 'NONE', #14571, 1000.000000000000000 ) ;
#17223 = PLANE ( 'NONE',  #13922 ) ;
#17224 = DIRECTION ( 'NONE',  ( -4.865963288531424442E-32, -6.824603186972751860E-48, -1.000000000000000000 ) ) ;
#17225 = CARTESIAN_POINT ( 'NONE',  ( -4.249412910294118717, 50.83092575845958550, 78.93669174070734584 ) ) ;
#17226 = DIRECTION ( 'NONE',  ( 1.000000000000000000, 2.838338907332122006E-16, -0.000000000000000000 ) ) ;
#17227 = CARTESIAN_POINT ( 'NONE',  ( 5.734785278855812685, 51.25223503655262647, 77.94915300234312383 ) ) ;
#17228 = CARTESIAN_POINT ( 'NONE',  ( -7.897028013293802218, 46.74808354956180523, 79.45433879953087342 ) ) ;
#17229 = DIRECTION ( 'NONE',  ( 1.540237394707284220E-16, 1.793354297423764243E-16, -1.000000000000000000 ) ) ;
#17230 = ORIENTED_EDGE ( 'NONE', *, *, #11092, .F. ) ;
#17231 = CARTESIAN_POINT ( 'NONE',  ( -4.348661956197086731, 37.56557963644259956, 78.93669174070734584 ) ) ;
#17232 = DIRECTION ( 'NONE',  ( -1.110223024625156540E-16, -1.000000000000000000, -5.922860397471808077E-17 ) ) ;
#17233 = DIRECTION ( 'NONE',  ( -0.5813877811927011807, 0.8136266022444372803, 5.636455622144619183E-17 ) ) ;
#17234 = CARTESIAN_POINT ( 'NONE',  ( -1.579458713576543882, 38.67424504380988282, 95.05433879952670395 ) ) ;
#17235 = LINE ( 'NONE', #17347, #6707 ) ;
#17236 = VECTOR ( 'NONE', #12843, 1000.000000000000000 ) ;
#17237 = CARTESIAN_POINT ( 'NONE',  ( -3.134114116279072437, 48.15229756555780227, 92.87621379611698558 ) ) ;
#17238 = LINE ( 'NONE', #2664, #7757 ) ;
#17239 = CARTESIAN_POINT ( 'NONE',  ( 6.828503391016846891, 43.33193468930419101, 92.75808880123800293 ) ) ;
#17240 = CARTESIAN_POINT ( 'NONE',  ( -4.397525688316068937, 51.46253079027765409, 76.14127734336351239 ) ) ;
#17241 = DIRECTION ( 'NONE',  ( -0.000000000000000000, -0.000000000000000000, 1.000000000000000000 ) ) ;
#17242 = CARTESIAN_POINT ( 'NONE',  ( -5.441938187485694911, 38.56320772136268715, 79.03330530165142420 ) ) ;
#17243 = EDGE_CURVE ( 'NONE', #6944, #5156, #14314, .T. ) ;
#17244 = VECTOR ( 'NONE', #15766, 1000.000000000000000 ) ;
#17245 = CARTESIAN_POINT ( 'NONE',  ( 0.8451174997408289480, 52.35581882004084520, 78.57205694827298714 ) ) ;
#17246 = VERTEX_POINT ( 'NONE', #9435 ) ;
#17247 = CARTESIAN_POINT ( 'NONE',  ( 1.920999019869927826, 52.24223821644631727, 75.80014879453128174 ) ) ;
#17248 = VERTEX_POINT ( 'NONE', #16028 ) ;
#17249 = VECTOR ( 'NONE', #980, 1000.000000000000000 ) ;
#17250 = CARTESIAN_POINT ( 'NONE',  ( -4.598246518171406727, 51.31910303412164609, 78.93669174070734584 ) ) ;
#17251 = B_SPLINE_CURVE_WITH_KNOTS ( 'NONE', 3,
 ( #14589, #116, #14692, #4578, #9498, #4996, #9396, #11515, #3208, #6182, #15985, #17569, #16088, #14378, #20853, #6281, #12782, #1728, #6490, #9811, #20949, #19369, #4783 ),
 .UNSPECIFIED., .F., .F.,
 ( 4, 2, 2, 2, 2, 2, 2, 2, 1, 2, 2, 4 ),
 ( 0.000000000000000000, 0.001314694893350534972, 0.001972042340025802459, 0.002629389786701069945, 0.003944084680051604917, 0.005258779573402139890, 0.006573474466752676597, 0.007230821913427943649, 0.007888169360103209835, 0.008545516806778478622, 0.009202864253453745674, 0.01051755914680430060 ),
 .UNSPECIFIED. ) ;
#17252 = CARTESIAN_POINT ( 'NONE',  ( 5.544968037009670780, 45.50804040601273925, 92.44558880294498238 ) ) ;
#17253 = EDGE_LOOP ( 'NONE', ( #3050, #16712, #28, #1046 ) ) ;
#17254 = CARTESIAN_POINT ( 'NONE',  ( 0.7901638384306279850, 50.30062182352762079, 93.57933879782396502 ) ) ;
#17255 = EDGE_CURVE ( 'NONE', #10941, #8009, #15922, .T. ) ;
#17256 = CARTESIAN_POINT ( 'NONE',  ( -0.5282253955477689278, 52.97542326866732054, 75.64626500862765113 ) ) ;
#17257 = DIRECTION ( 'NONE',  ( 5.626130192357176673E-16, 1.831515347669941892E-30, -1.000000000000000000 ) ) ;
#17258 = CARTESIAN_POINT ( 'NONE',  ( 0.5221537403065010796, 44.16218137147969003, 77.84651775085080772 ) ) ;
#17259 = SURFACE_SIDE_STYLE ('',( #14377 ) ) ;
#17260 = DIRECTION ( 'NONE',  ( 1.084202172485505420E-16, 1.000000000000000000, 0.000000000000000000 ) ) ;
#17261 = ORIENTED_EDGE ( 'NONE', *, *, #1603, .T. ) ;
#17262 = CARTESIAN_POINT ( 'NONE',  ( 2.259191861956064251, 47.76843358786783256, 85.41730067788145675 ) ) ;
#17263 = AXIS2_PLACEMENT_3D ( 'NONE', #12670, #18937, #2974 ) ;
#17264 = ORIENTED_EDGE ( 'NONE', *, *, #18475, .T. ) ;
#17265 = CARTESIAN_POINT ( 'NONE',  ( 9.539487329945091076, 44.16218137147969713, 73.00433879953099847 ) ) ;
#17266 = CARTESIAN_POINT ( 'NONE',  ( 5.241460166982748525, 50.86801069014953924, 78.59183879953087626 ) ) ;
#17267 = PLANE ( 'NONE',  #950 ) ;
#17268 = CARTESIAN_POINT ( 'NONE',  ( 5.611423337425062385, 41.22389019960463230, 95.17996380123798872 ) ) ;
#17269 = CARTESIAN_POINT ( 'NONE',  ( 9.273778039597953438, 45.67340037358405169, 78.74919174070734584 ) ) ;
#17270 = CARTESIAN_POINT ( 'NONE',  ( -4.285954277864442830, 37.51963121091066711, 77.94459252611197542 ) ) ;
#17271 = CARTESIAN_POINT ( 'NONE',  ( 5.126612573611699197, 37.37671407926408307, 78.18547655874309044 ) ) ;
#17272 = VERTEX_POINT ( 'NONE', #1446 ) ;
#17273 = CARTESIAN_POINT ( 'NONE',  ( 0.5221537403065107386, 50.16218137147969713, 53.15433879953100416 ) ) ;
#17274 = VECTOR ( 'NONE', #780, 1000.000000000000227 ) ;
#17275 = ORIENTED_EDGE ( 'NONE', *, *, #1836, .T. ) ;
#17276 = CARTESIAN_POINT ( 'NONE',  ( 10.77494014480653561, 42.96218137147968008, 77.80433879953099563 ) ) ;
#17277 = CARTESIAN_POINT ( 'NONE',  ( 3.460444912181559474, 49.25145096859824889, 93.14871380123798872 ) ) ;
#17278 = CARTESIAN_POINT ( 'NONE',  ( 5.159368991072407873, 51.67727186915629289, 75.44114465464750197 ) ) ;
#17279 = VERTEX_POINT ( 'NONE', #361 ) ;
#17280 = CARTESIAN_POINT ( 'NONE',  ( 2.043125170982144745, 38.48583871533720213, 92.67996380123798872 ) ) ;
#17281 = CARTESIAN_POINT ( 'NONE',  ( -5.261478123908109872, 50.84518201112111058, 79.40394833312912226 ) ) ;
#17282 = CARTESIAN_POINT ( 'NONE',  ( 30.92220646078100188, 42.76218137147968434, 56.80715055817104542 ) ) ;
#17283 = DIRECTION ( 'NONE',  ( 1.000000000000000000, 0.000000000000000000, 0.000000000000000000 ) ) ;
#17284 = EDGE_CURVE ( 'NONE', #2386, #6017, #19615, .T. ) ;
#17285 = CARTESIAN_POINT ( 'NONE',  ( 42.52215374030651418, 40.36218137147969287, 45.55432679953101172 ) ) ;
#17286 = EDGE_LOOP ( 'NONE', ( #480, #7882, #1818, #12881 ) ) ;
#17287 = CARTESIAN_POINT ( 'NONE',  ( -1.077846259693493680, 47.82824192744436687, 61.55433879953100273 ) ) ;
#17288 = CARTESIAN_POINT ( 'NONE',  ( 0.6268041787565157286, 52.35390056590507868, 78.93480014378108933 ) ) ;
#17289 = EDGE_LOOP ( 'NONE', ( #18856, #2860, #9670, #19929 ) ) ;
#17290 = FACE_OUTER_BOUND ( 'NONE', #12298, .T. ) ;
#17291 = CARTESIAN_POINT ( 'NONE',  ( -0.4699484075729999932, 51.36218137147968577, 83.03825919817350609 ) ) ;
#17292 = CARTESIAN_POINT ( 'NONE',  ( 5.856396280011939126, 46.10368687828906076, 94.59496379782397923 ) ) ;
#17293 = VECTOR ( 'NONE', #9168, 1000.000000000000000 ) ;
#17294 = ITEM_DEFINED_TRANSFORMATION ( 'NONE', 'NONE', #3743,  #18366 ) ;
#17295 = CARTESIAN_POINT ( 'NONE',  ( 5.431844598077052666, 36.85469448565577011, 76.44059830477070250 ) ) ;
#17297 = ADVANCED_FACE ( 'NONE', ( #11557 ), #6849, .F. ) ;
#17296 = CARTESIAN_POINT ( 'NONE',  ( 5.658108625003792191, 37.01637447524286273, 75.97198585835440099 ) ) ;
#17298 = FACE_OUTER_BOUND ( 'NONE', #5572, .T. ) ;
#17299 = ADVANCED_FACE ( 'NONE', ( #19725 ), #3453, .T. ) ;
#17300 = ORIENTED_EDGE ( 'NONE', *, *, #9609, .F. ) ;
#17301 = CARTESIAN_POINT ( 'NONE',  ( 2.008116822278622760, 52.95519856864822827, 75.93722239247614425 ) ) ;
#17302 = ORIENTED_EDGE ( 'NONE', *, *, #19596, .T. ) ;
#17303 = CARTESIAN_POINT ( 'NONE',  ( -1.077846259693493458, 50.16218137147969713, 61.55433879953100273 ) ) ;
#17304 = ADVANCED_FACE ( 'NONE', ( #3658 ), #8567, .F. ) ;
#17305 = CARTESIAN_POINT ( 'NONE',  ( -0.2332032163833130112, 52.32814213131982939, 75.48592037115906805 ) ) ;
#17306 = CARTESIAN_POINT ( 'NONE',  ( 1.352400422481993658, 50.46853102219002096, 90.72683880123797451 ) ) ;
#17307 = EDGE_CURVE ( 'NONE', #12777, #5789, #18396, .T. ) ;
#17308 = CARTESIAN_POINT ( 'NONE',  ( 11.22215374030649926, 48.36218137147968577, 80.55433879953099563 ) ) ;
#17309 = ORIENTED_EDGE ( 'NONE', *, *, #11991, .F. ) ;
#17310 = VECTOR ( 'NONE', #3538, 1000.000000000000000 ) ;
#17311 = CARTESIAN_POINT ( 'NONE',  ( -3.557579061748612048, 36.23530104570325250, 76.03954924220039402 ) ) ;
#17312 = CARTESIAN_POINT ( 'NONE',  ( 0.3869120917952214023, 35.96329670974014192, 75.45433879953087342 ) ) ;
#17313 = ORIENTED_EDGE ( 'NONE', *, *, #10762, .F. ) ;
#17314 = EDGE_CURVE ( 'NONE', #496, #4878, #5142, .T. ) ;
#17315 = CARTESIAN_POINT ( 'NONE',  ( 5.319542448682613944, 51.55895818820005871, 79.51138782552760631 ) ) ;
#17316 =( BOUNDED_CURVE ( )  B_SPLINE_CURVE ( 3, ( #3785, #11890, #13574, #18257 ),
 .UNSPECIFIED., .F., .F. ) 
 B_SPLINE_CURVE_WITH_KNOTS ( ( 4, 4 ),
 ( 5.006904465492826084, 5.052225889838809714 ),
 .UNSPECIFIED. ) 
 CURVE ( )  GEOMETRIC_REPRESENTATION_ITEM ( )  RATIONAL_B_SPLINE_CURVE ( ( 1.000000000000000000, 0.9998288380325438540, 0.9998288380325438540, 1.000000000000000000 ) ) 
 REPRESENTATION_ITEM ( '' )  );
#17317 = DIRECTION ( 'NONE',  ( -1.000000000000000000, 0.000000000000000000, 0.000000000000000000 ) ) ;
#17318 = CARTESIAN_POINT ( 'NONE',  ( -1.590937568396968649, 39.63064243629642647, 91.07933879953097289 ) ) ;
#17319 = AXIS2_PLACEMENT_3D ( 'NONE', #13067, #12652, #9463 ) ;
#17320 = ORIENTED_EDGE ( 'NONE', *, *, #17130, .T. ) ;
#17321 = CARTESIAN_POINT ( 'NONE',  ( 6.521955874970234213, 49.75166928465916527, 76.54279163422609145 ) ) ;
#17322 = CARTESIAN_POINT ( 'NONE',  ( -6.796670188453681760, 40.58727050948505166, 79.17963929739188700 ) ) ;
#17323 = CYLINDRICAL_SURFACE ( 'NONE', #4161, 1.399999999999998579 ) ;
#17324 = CARTESIAN_POINT ( 'NONE',  ( 6.828503391016846891, 43.33193468930419101, 91.66433880123796030 ) ) ;
#17325 = DIRECTION ( 'NONE',  ( -1.110223024625156540E-16, -1.000000000000000000, -5.922860397471808077E-17 ) ) ;
#17326 = VECTOR ( 'NONE', #18247, 1000.000000000000000 ) ;
#17327 = CARTESIAN_POINT ( 'NONE',  ( 4.638945281793899866, 51.13685495226798139, 75.47011219584838670 ) ) ;
#17328 = CARTESIAN_POINT ( 'NONE',  ( 3.122153740306552905, 48.66551347115873227, 95.10183880294498238 ) ) ;
#17329 = VECTOR ( 'NONE', #13607, 1000.000000000000227 ) ;
#17330 = CARTESIAN_POINT ( 'NONE',  ( -7.409257659412860519, 40.34942259774520323, 79.14159390612334732 ) ) ;
#17331 = SURFACE_SIDE_STYLE ('',( #6040 ) ) ;
#17332 = CARTESIAN_POINT ( 'NONE',  ( -0.9375046559398532153, 52.97987584641302305, 77.82884852524264829 ) ) ;
#17333 = DIRECTION ( 'NONE',  ( -0.000000000000000000, 1.000000000000000000, -0.000000000000000000 ) ) ;
#17334 = CARTESIAN_POINT ( 'NONE',  ( 0.3279640439667353413, 52.35988168082470651, 72.45433879953087342 ) ) ;
#17335 = EDGE_CURVE ( 'NONE', #2175, #2442, #157, .T. ) ;
#17336 = CARTESIAN_POINT ( 'NONE',  ( -4.383473025373059606, 51.47257230871590394, 78.45066232894264147 ) ) ;
#17337 = CARTESIAN_POINT ( 'NONE',  ( -2.416137431568557314, 39.07291177436112406, 91.27371380123798872 ) ) ;
#17338 = CARTESIAN_POINT ( 'NONE',  ( -7.222486564444017709, 46.56685618261736437, 79.41298732254628590 ) ) ;
#17339 = CARTESIAN_POINT ( 'NONE',  ( 5.428747419638988880, 36.85248135533887393, 77.49967648550449439 ) ) ;
#17340 = AXIS2_PLACEMENT_3D ( 'NONE', #10954, #6340, #9673 ) ;
#17341 = AXIS2_PLACEMENT_3D ( 'NONE', #4803, #11322, #5995 ) ;
#17342 = CARTESIAN_POINT ( 'NONE',  ( 7.978846747739011036, 40.74910683537441258, 75.50210680925209772 ) ) ;
#17343 = CARTESIAN_POINT ( 'NONE',  ( -4.036988424348830762, 50.97791528042453990, 76.24981967119607873 ) ) ;
#17344 = DIRECTION ( 'NONE',  ( 1.110223024625156294E-16, -1.000000000000000000, -7.183611964723542594E-17 ) ) ;
#17345 = DIRECTION ( 'NONE',  ( -0.000000000000000000, -0.000000000000000000, 1.000000000000000000 ) ) ;
#17346 = B_SPLINE_SURFACE_WITH_KNOTS ( 'NONE', 3, 1, ( 
 ( #12460, #1082 ),
 ( #17144, #13838 ),
 ( #20318, #12562 ),
 ( #2565, #4466 ),
 ( #10778, #17460 ),
 ( #17242, #10569 ),
 ( #4156, #6479 ),
 ( #12771, #19563 ),
 ( #14679, #19155 ),
 ( #104, #8189 ),
 ( #17769, #20937 ),
 ( #4566, #360 ),
 ( #1604, #6584 ),
 ( #11186, #19250 ),
 ( #3292, #9700 ),
 ( #17869, #16179 ),
 ( #14365, #4662 ),
 ( #20842, #17655 ),
 ( #3196, #6269 ) ),
 .UNSPECIFIED., .F., .F., .F.,
 ( 4, 1, 1, 1, 1, 1, 1, 1, 1, 1, 1, 1, 1, 1, 1, 1, 4 ),
 ( 2, 2 ),
 ( 0.000000000000000000, 0.07046818618994758754, 0.1352139183126853383, 0.1951004221781245107, 0.2505542266086520642, 0.3026661728221104464, 0.3524186183690131702, 0.4011907228821319227, 0.4500572973727005044, 0.5012199576353847386, 0.5567639849620312775, 0.6168130928284528691, 0.6819767269214894734, 0.7529340711039560485, 0.8292206168931396393, 0.9117786016023526896, 1.000000000000000000 ),
 ( 0.000000000000000000, 1.000000000000000000 ),
 .UNSPECIFIED. ) ;
#17347 = CARTESIAN_POINT ( 'NONE',  ( 8.832380548758539618, 43.45507459029314390, 95.45352954694192249 ) ) ;
#17348 = CIRCLE ( 'NONE', #699, 8.199999999999995737 ) ;
#17349 = CARTESIAN_POINT ( 'NONE',  ( -4.042113542615705768, 50.97449326430325556, 78.71838125468477187 ) ) ;
#17350 = DIRECTION ( 'NONE',  ( -1.402518428993831183E-16, 1.000000000000000000, -3.469446951953617640E-16 ) ) ;
#17351 = EDGE_LOOP ( 'NONE', ( #1875, #1216, #20571, #15488 ) ) ;
#17352 = CARTESIAN_POINT ( 'NONE',  ( -5.154188915835984375, 42.64120994080404614, 90.96121380123797451 ) ) ;
#17353 = TOROIDAL_SURFACE ( 'NONE', #8175, 13.99999999999999645, 4.000000000000000000 ) ;
#17354 = CARTESIAN_POINT ( 'NONE',  ( -5.510796958474739604, 38.60848837797752964, 77.05433879953086773 ) ) ;
#17355 = ORIENTED_EDGE ( 'NONE', *, *, #1938, .T. ) ;
#17356 = CARTESIAN_POINT ( 'NONE',  ( 2.107928617576430241, 52.20740276032782390, 76.30768396657595076 ) ) ;
#17357 = ORIENTED_EDGE ( 'NONE', *, *, #8741, .F. ) ;
#17358 = CARTESIAN_POINT ( 'NONE',  ( -7.600593896485820622, 45.28511094584521146, 72.45433879953085921 ) ) ;
#17359 = CARTESIAN_POINT ( 'NONE',  ( -0.8237052942265477018, 49.18499566818285018, 90.25808880294496817 ) ) ;
#17360 = ORIENTED_EDGE ( 'NONE', *, *, #16483, .T. ) ;
#17361 = CARTESIAN_POINT ( 'NONE',  ( -4.622577041588897373, 46.56120873422322859, 93.81371379782397923 ) ) ;
#17362 = CARTESIAN_POINT ( 'NONE',  ( -0.9377844550628051667, 52.97865279236703628, 77.21536821129558348 ) ) ;
#17363 = CARTESIAN_POINT ( 'NONE',  ( 8.644901377098817008, 43.03925179711409754, 72.45433879953087342 ) ) ;
#17364 = CARTESIAN_POINT ( 'NONE',  ( 0.5221537403065100724, 44.16218137147969713, 53.55433879953100273 ) ) ;
#17365 = DIRECTION ( 'NONE',  ( 0.007885122365275663500, 0.9999689119394085113, 1.805443505845543142E-16 ) ) ;
#17366 = ORIENTED_EDGE ( 'NONE', *, *, #3395, .F. ) ;
#17367 =( GEOMETRIC_REPRESENTATION_CONTEXT ( 3 ) GLOBAL_UNCERTAINTY_ASSIGNED_CONTEXT ( ( #17026 ) ) GLOBAL_UNIT_ASSIGNED_CONTEXT ( ( #13373, #18255, #11579 ) ) REPRESENTATION_CONTEXT ( 'NONE', 'WORKASPACE' ) );
#17368 = DIRECTION ( 'NONE',  ( 1.540237394707284220E-16, 1.793354297423764243E-16, -1.000000000000000000 ) ) ;
#17369 = EDGE_CURVE ( 'NONE', #585, #15690, #3346, .T. ) ;
#17370 = ORIENTED_EDGE ( 'NONE', *, *, #268, .F. ) ;
#17371 = CARTESIAN_POINT ( 'NONE',  ( 2.522153740306511516, 50.16218137147969713, 50.55433879953100273 ) ) ;
#17372 = DIRECTION ( 'NONE',  ( 1.540237394707284220E-16, 1.793354297423764243E-16, -1.000000000000000000 ) ) ;
#17373 = CARTESIAN_POINT ( 'NONE',  ( 5.497743849324332466, 37.64424434608246628, 76.58742703482498371 ) ) ;
#17374 = CARTESIAN_POINT ( 'NONE',  ( 4.359773538758245692, 47.36728266200564263, 95.05433879953096721 ) ) ;
#17375 = CARTESIAN_POINT ( 'NONE',  ( 5.666884522201894647, 41.76315400873614436, 94.43871379782397923 ) ) ;
#17376 = LINE ( 'NONE', #13865, #20778 ) ;
#17377 = AXIS2_PLACEMENT_3D ( 'NONE', #18609, #8724, #5728 ) ;
#17378 = ORIENTED_EDGE ( 'NONE', *, *, #13517, .F. ) ;
#17379 = CARTESIAN_POINT ( 'NONE',  ( 8.284178787249310005, 41.51768607177196913, 75.97387361979315301 ) ) ;
#17380 = AXIS2_PLACEMENT_3D ( 'NONE', #13353, #18341, #3559 ) ;
#17381 = VERTEX_POINT ( 'NONE', #11661 ) ;
#17382 = CARTESIAN_POINT ( 'NONE',  ( -4.089052737068717747, 51.68295426732343856, 75.42336258079946276 ) ) ;
#17383 = CARTESIAN_POINT ( 'NONE',  ( 1.352400422481993658, 50.46853102219002096, 94.47683880123798872 ) ) ;
#17384 = B_SPLINE_CURVE_WITH_KNOTS ( 'NONE', 3,
 ( #898, #7172, #13671, #7386, #20146, #10501, #16966, #15385, #2396, #8898 ),
 .UNSPECIFIED., .F., .F.,
 ( 4, 2, 2, 2, 4 ),
 ( 0.000000000000000000, 0.0001324019452384074113, 0.0002648038904768148225, 0.0003972058357152222609, 0.0005296077809536294282 ),
 .UNSPECIFIED. ) ;
#17385 = CARTESIAN_POINT ( 'NONE',  ( -7.785946528631249919, 41.22915307650257688, 78.55785233681892521 ) ) ;
#17386 = ORIENTED_EDGE ( 'NONE', *, *, #20989, .T. ) ;
#17387 = CARTESIAN_POINT ( 'NONE',  ( -5.528784567355424784, 50.65417461334718752, 79.23104009678212378 ) ) ;
#17388 = CARTESIAN_POINT ( 'NONE',  ( 19.23948732994503885, 45.16218137147969003, 84.70433879953101552 ) ) ;
#17389 = EDGE_LOOP ( 'NONE', ( #11123, #2136, #12624, #10451 ) ) ;
#17390 = CARTESIAN_POINT ( 'NONE',  ( 6.880715602165139444, 37.89000465862396538, 77.41265765549051991 ) ) ;
#17391 = CARTESIAN_POINT ( 'NONE',  ( -4.137897255279099795, 50.90113633070201615, 78.91875292420674270 ) ) ;
#17392 = EDGE_CURVE ( 'NONE', #17442, #6443, #5037, .T. ) ;
#17393 = ORIENTED_EDGE ( 'NONE', *, *, #6628, .T. ) ;
#17394 = CARTESIAN_POINT ( 'NONE',  ( -0.3080929418689875576, 37.85583172076933778, 91.35183880123798872 ) ) ;
#17395 = AXIS2_PLACEMENT_3D ( 'NONE', #19728, #11354, #160 ) ;
#17396 = VERTEX_POINT ( 'NONE', #15054 ) ;
#17397 = CARTESIAN_POINT ( 'NONE',  ( -3.233102370063162034, 40.36700684672312889, 92.45433879953093026 ) ) ;
#17398 = FACE_OUTER_BOUND ( 'NONE', #14706, .T. ) ;
#17399 = AXIS2_PLACEMENT_3D ( 'NONE', #13929, #20410, #17438 ) ;
#17400 = CARTESIAN_POINT ( 'NONE',  ( -3.628867371436362621, 48.69222599884265179, 91.23558879782397923 ) ) ;
#17401 = CARTESIAN_POINT ( 'NONE',  ( 5.428282431822193388, 36.85214909206928269, 76.61095391776262886 ) ) ;
#17402 = CARTESIAN_POINT ( 'NONE',  ( 5.268505869694503296, 50.84354137661855333, 78.86786983087660019 ) ) ;
#17403 = CARTESIAN_POINT ( 'NONE',  ( -3.405066831027640184, 37.04747935142366089, 77.64672866243046201 ) ) ;
#17404 = ADVANCED_FACE ( 'NONE', ( #8248 ), #13294, .T. ) ;
#17405 = ORIENTED_EDGE ( 'NONE', *, *, #16136, .T. ) ;
#17406 = CARTESIAN_POINT ( 'NONE',  ( 2.119851040271390374, 52.81592988514039178, 77.84551527011910821 ) ) ;
#17407 = ORIENTED_EDGE ( 'NONE', *, *, #7390, .F. ) ;
#17408 = VECTOR ( 'NONE', #17760, 1000.000000000000000 ) ;
#17409 = CARTESIAN_POINT ( 'NONE',  ( 6.848903495604322877, 50.42928078925980628, 75.87133531663224062 ) ) ;
#17410 = CARTESIAN_POINT ( 'NONE',  ( 0.1157200918968281783, 52.35296189364724739, 75.39535632244431440 ) ) ;
#17411 = CARTESIAN_POINT ( 'NONE',  ( 3.460444912181559474, 49.25145096859824889, 95.49246380123798872 ) ) ;
#17412 = VECTOR ( 'NONE', #9606, 1000.000000000000227 ) ;
#17413 = DIRECTION ( 'NONE',  ( -0.5941461771851691553, -0.8043570849667760481, -2.357623395011396791E-16 ) ) ;
#17414 = EDGE_LOOP ( 'NONE', ( #796, #2675, #12742, #20321 ) ) ;
#17415 = VERTEX_POINT ( 'NONE', #6605 ) ;
#17416 = CARTESIAN_POINT ( 'NONE',  ( -3.709553250900186061, 37.27239120432235353, 75.43521673441158271 ) ) ;
#17417 = CARTESIAN_POINT ( 'NONE',  ( -6.920926855474425210, 40.72042203567113461, 77.43482967097732228 ) ) ;
#17418 = ORIENTED_EDGE ( 'NONE', *, *, #13643, .F. ) ;
#17419 = CARTESIAN_POINT ( 'NONE',  ( 4.676321589340446394, 52.03407952647943091, 79.02133806855546538 ) ) ;
#17420 = EDGE_CURVE ( 'NONE', #10020, #3468, #3628, .T. ) ;
#17421 = DIRECTION ( 'NONE',  ( -0.3165065846431827645, -0.9485903129789529098, 0.000000000000000000 ) ) ;
#17422 = CARTESIAN_POINT ( 'NONE',  ( -3.134114116279071549, 48.15229756555780227, 91.93871379953098710 ) ) ;
#17423 = EDGE_CURVE ( 'NONE', #11304, #13330, #17892, .T. ) ;
#17424 = ORIENTED_EDGE ( 'NONE', *, *, #16638, .F. ) ;
#17425 = CARTESIAN_POINT ( 'NONE',  ( -4.608953993764351331, 37.01190935601766085, 77.97288938838475758 ) ) ;
#17426 = CARTESIAN_POINT ( 'NONE',  ( 5.900862589321786977, 51.12956041731354873, 78.19629421043239859 ) ) ;
#17427 = CARTESIAN_POINT ( 'NONE',  ( -5.312295682859165424, 38.39999490510201952, 79.30838064730033921 ) ) ;
#17428 = CARTESIAN_POINT ( 'NONE',  ( 6.198496396448986090, 45.68315280215533392, 95.33621380123798872 ) ) ;
#17429 = VECTOR ( 'NONE', #6203, 1000.000000000000000 ) ;
#17430 = VECTOR ( 'NONE', #14578, 1000.000000000000114 ) ;
#17431 = EDGE_CURVE ( 'NONE', #9854, #7365, #16199, .T. ) ;
#17432 = CARTESIAN_POINT ( 'NONE',  ( -5.170918566808907713, 50.90989255502720567, 75.43678921887351407 ) ) ;
#17433 = DIRECTION ( 'NONE',  ( -1.000000000000000000, 1.193617070626243484E-16, 0.000000000000000000 ) ) ;
#17434 = DIRECTION ( 'NONE',  ( 1.110223024625156540E-16, 1.000000000000000000, 5.922860397471808077E-17 ) ) ;
#17435 = CARTESIAN_POINT ( 'NONE',  ( -0.3533744273842052697, 52.21282903393489505, 79.37504392981026058 ) ) ;
#17436 = ORIENTED_EDGE ( 'NONE', *, *, #18098, .F. ) ;
#17437 = DIRECTION ( 'NONE',  ( -0.4999999999999984457, -0.8660254037844394848, -0.000000000000000000 ) ) ;
#17438 = DIRECTION ( 'NONE',  ( 1.000000000000000000, 0.000000000000000000, 0.000000000000000000 ) ) ;
#17439 = CARTESIAN_POINT ( 'NONE',  ( 0.8457835444558534643, 52.35579252807401929, 76.43141481149322658 ) ) ;
#17440 = LINE ( 'NONE', #7864, #6844 ) ;
#17441 =( BOUNDED_CURVE ( )  B_SPLINE_CURVE ( 3, ( #4042, #15660, #2666, #10568 ),
 .UNSPECIFIED., .F., .T. ) 
 B_SPLINE_CURVE_WITH_KNOTS ( ( 4, 4 ),
 ( 5.988669822071448934, 6.577700792287723530 ),
 .UNSPECIFIED. ) 
 CURVE ( )  GEOMETRIC_REPRESENTATION_ITEM ( )  RATIONAL_B_SPLINE_CURVE ( ( 1.000000000000000000, 0.9712952651971044071, 0.9712952651971044071, 1.000000000000000000 ) ) 
 REPRESENTATION_ITEM ( '' )  );
#17442 = VERTEX_POINT ( 'NONE', #18001 ) ;
#17443 = AXIS2_PLACEMENT_3D ( 'NONE', #18589, #8921, #13390 ) ;
#17444 = CARTESIAN_POINT ( 'NONE',  ( -7.999076009197850112, 41.90847905551897412, 79.52797380487967871 ) ) ;
#17445 = CARTESIAN_POINT ( 'NONE',  ( 5.694963103159264683, 37.04270933600420079, 75.97340568087561508 ) ) ;
#17446 = VERTEX_POINT ( 'NONE', #9934 ) ;
#17447 = CARTESIAN_POINT ( 'NONE',  ( 8.637769616985924159, 43.04608606469359700, 78.67881838835081965 ) ) ;
#17449 = EDGE_CURVE ( 'NONE', #19468, #4403, #16620, .T. ) ;
#17448 = DIRECTION ( 'NONE',  ( 0.007885122365275663500, 0.9999689119394085113, 1.805443505845543142E-16 ) ) ;
#17450 = CARTESIAN_POINT ( 'NONE',  ( 4.621588727139584130, 51.26391586304784198, 77.68963291717793140 ) ) ;
#17451 = CYLINDRICAL_SURFACE ( 'NONE', #14050, 4.199999999999999289 ) ;
#17452 = DIRECTION ( 'NONE',  ( -1.000000000000000000, 0.000000000000000000, 0.000000000000000000 ) ) ;
#17453 = CARTESIAN_POINT ( 'NONE',  ( 9.035997676120972599, 41.87518277052537030, 78.13634973986094678 ) ) ;
#17454 = CARTESIAN_POINT ( 'NONE',  ( 10.77494014480653561, 42.96218137147968008, 69.40574467885102194 ) ) ;
#17455 = CARTESIAN_POINT ( 'NONE',  ( 5.203359478703453611, 50.89466331855276593, 76.29855684506968316 ) ) ;
#17456 = EDGE_CURVE ( 'NONE', #3130, #7921, #2931, .T. ) ;
#17457 = EDGE_CURVE ( 'NONE', #9334, #8809, #17035, .T. ) ;
#17458 = VECTOR ( 'NONE', #6683, 1000.000000000000000 ) ;
#17459 = EDGE_LOOP ( 'NONE', ( #7280, #5143, #789, #8862 ) ) ;
#17460 = CARTESIAN_POINT ( 'NONE',  ( -5.919594526472896412, 37.98002672170838423, 78.92638042842689572 ) ) ;
#17461 = CARTESIAN_POINT ( 'NONE',  ( -4.574316323987747346, 51.33620267474496757, 79.54845644658969661 ) ) ;
#17462 = DIRECTION ( 'NONE',  ( 0.000000000000000000, 0.000000000000000000, 1.000000000000000000 ) ) ;
#17463 = VERTEX_POINT ( 'NONE', #25 ) ;
#17464 = CARTESIAN_POINT ( 'NONE',  ( 28.52215374030649642, 44.16218137147969003, 87.05433879953100984 ) ) ;
#17465 = CARTESIAN_POINT ( 'NONE',  ( 1.868012774839550749, 39.13936707477651566, 90.88308880294496817 ) ) ;
#17466 = ORIENTED_EDGE ( 'NONE', *, *, #6078, .F. ) ;
#17467 = CARTESIAN_POINT ( 'NONE',  ( 5.527130473740349714, 50.65250579964440902, 78.81551702238962775 ) ) ;
#17468 = LINE ( 'NONE', #15782, #18640 ) ;
#17469 = CARTESIAN_POINT ( 'NONE',  ( 5.389492195292208798, 36.82443100924615464, 78.79551527011911105 ) ) ;
#17470 = DIRECTION ( 'NONE',  ( 1.402518428993831676E-16, -1.000000000000000000, -0.000000000000000000 ) ) ;
#17471 = CARTESIAN_POINT ( 'NONE',  ( 0.7579357306838750974, 52.35285379749892343, 76.01945459498423929 ) ) ;
#17472 = CARTESIAN_POINT ( 'NONE',  ( -3.437559636576261290, 37.06066253623392726, 79.33401574558745040 ) ) ;
#17473 = ORIENTED_EDGE ( 'NONE', *, *, #2765, .T. ) ;
#17474 = CARTESIAN_POINT ( 'NONE',  ( 5.631785411401764918, 36.99756487055721976, 77.76022115247205591 ) ) ;
#17475 = CARTESIAN_POINT ( 'NONE',  ( 0.2541436421823711211, 38.02374091943176637, 92.79808879782397923 ) ) ;
#17476 = EDGE_LOOP ( 'NONE', ( #13155, #15650, #9472, #6598 ) ) ;
#17477 = CARTESIAN_POINT ( 'NONE',  ( -4.567115856812060670, 47.10047254335474065, 93.30496380123798872 ) ) ;
#17478 = EDGE_CURVE ( 'NONE', #158, #17483, #16516, .T. ) ;
#17479 = CARTESIAN_POINT ( 'NONE',  ( -4.567115856812060670, 47.10047254335474065, 94.55496380123798872 ) ) ;
#17480 = FACE_OUTER_BOUND ( 'NONE', #190, .T. ) ;
#17481 = CARTESIAN_POINT ( 'NONE',  ( -4.812088799398940075, 42.22067586467031930, 95.21996379782397923 ) ) ;
#17482 = LINE ( 'NONE', #6289, #16385 ) ;
#17483 = VERTEX_POINT ( 'NONE', #19484 ) ;
#17484 = CARTESIAN_POINT ( 'NONE',  ( 4.577678780824717464, 52.10694299555530051, 78.38317481739672132 ) ) ;
#17485 = ORIENTED_EDGE ( 'NONE', *, *, #20291, .F. ) ;
#17486 = CARTESIAN_POINT ( 'NONE',  ( -3.471062581449894768, 51.20477182418656525, 75.48713596493043099 ) ) ;
#17487 = CARTESIAN_POINT ( 'NONE',  ( 5.025485839985549319, 41.56218137147963887, 90.72683879953099506 ) ) ;
#17488 = CARTESIAN_POINT ( 'NONE',  ( 4.694131320935415630, 52.02092419516998234, 75.77039595153209461 ) ) ;
#17489 = ORIENTED_EDGE ( 'NONE', *, *, #15769, .F. ) ;
#17490 = CARTESIAN_POINT ( 'NONE',  ( -5.569761608070843195, 50.62489392031717728, 79.19259575086972802 ) ) ;
#17491 = EDGE_LOOP ( 'NONE', ( #13771, #1081, #4173, #6060, #19522, #2545 ) ) ;
#17492 = CARTESIAN_POINT ( 'NONE',  ( 5.116981105040771638, 36.62970456142029008, 75.43572969368668168 ) ) ;
#17493 = EDGE_CURVE ( 'NONE', #7818, #9780, #19405, .T. ) ;
#17494 = CARTESIAN_POINT ( 'NONE',  ( -4.098212357736016109, 50.92949370552946675, 78.89116106075270807 ) ) ;
#17495 = EDGE_LOOP ( 'NONE', ( #1415, #11338, #17424, #11072, #14020 ) ) ;
#17496 = CARTESIAN_POINT ( 'NONE',  ( 5.722153740305850000, 42.76884557083668881, 93.27737681315549878 ) ) ;
#17497 = FACE_OUTER_BOUND ( 'NONE', #9312, .T. ) ;
#17498 = ORIENTED_EDGE ( 'NONE', *, *, #10319, .T. ) ;
#17499 = FACE_OUTER_BOUND ( 'NONE', #13840, .T. ) ;
#17500 = CARTESIAN_POINT ( 'NONE',  ( 4.685659163076279832, 40.18527142738543745, 95.05433879953100984 ) ) ;
#17501 = CARTESIAN_POINT ( 'NONE',  ( 4.673174852049361228, 39.63213674411673537, 94.36058879782399345 ) ) ;
#17502 = CARTESIAN_POINT ( 'NONE',  ( 5.618638386382252214, 36.98817048782158423, 75.97391373086902888 ) ) ;
#17503 = CARTESIAN_POINT ( 'NONE',  ( 8.807466118993687587, 41.19025919604325026, 76.04813117819971069 ) ) ;
#17504 = CARTESIAN_POINT ( 'NONE',  ( -3.269283392368544927, 36.94718159497673327, 77.55767546204062057 ) ) ;
#17505 = ORIENTED_EDGE ( 'NONE', *, *, #20258, .T. ) ;
#17506 = CARTESIAN_POINT ( 'NONE',  ( 2.097007766388983008, 52.95433544280876248, 78.67719617274387645 ) ) ;
#17507 = CARTESIAN_POINT ( 'NONE',  ( 5.562039828671766273, 37.70552590032356477, 78.36928251986560667 ) ) ;
#17508 = CARTESIAN_POINT ( 'NONE',  ( -3.847046057864465851, 36.44911865529216755, 77.75315568452884918 ) ) ;
#17509 = EDGE_CURVE ( 'NONE', #1203, #6639, #18209, .T. ) ;
#17510 = EDGE_LOOP ( 'NONE', ( #1831, #8701, #14709, #6090, #14890, #18897, #13559, #13103, #3787, #19733, #9531, #16621, #14811, #11414, #633, #20576, #6823, #8990, #18267, #20275, #2555, #9024, #13905, #20471, #16511, #18258, #16215 ) ) ;
#17511 = CARTESIAN_POINT ( 'NONE',  ( -7.794114027700602243, 41.28466036262712890, 78.36261600855591780 ) ) ;
#17512 = CARTESIAN_POINT ( 'NONE',  ( 5.495636600878563982, 37.64719334750368063, 77.37492703482499223 ) ) ;
#17513 = CARTESIAN_POINT ( 'NONE',  ( -4.524181921268124462, 40.28999182795290324, 94.78933880123798872 ) ) ;
#17514 = B_SPLINE_SURFACE_WITH_KNOTS ( 'NONE', 3, 1, ( 
 ( #18854, #3852 ),
 ( #15250, #4266 ),
 ( #16943, #2370 ),
 ( #10793, #10373 ),
 ( #16843, #7145 ),
 ( #13649, #18541 ),
 ( #15785, #16087 ),
 ( #4370, #20644 ),
 ( #1510, #11099 ),
 ( #7785, #12781 ),
 ( #14266, #6074 ),
 ( #11000, #20747 ),
 ( #12685, #9296 ),
 ( #17471, #4782 ),
 ( #1296, #10896 ),
 ( #17670, #7996 ),
 ( #3102, #12579 ),
 ( #2895, #19069 ),
 ( #6181, #9605 ) ),
 .UNSPECIFIED., .F., .F., .F.,
 ( 4, 1, 1, 1, 1, 1, 1, 1, 1, 1, 1, 1, 1, 1, 1, 1, 4 ),
 ( 2, 2 ),
 ( 0.000000000000000000, 0.09451313814127135227, 0.1805372682721389788, 0.2570047093480871125, 0.3249775091219202494, 0.3834231080405892667, 0.4323187449081173361, 0.4717396676274380751, 0.5027004295337662576, 0.5542129903573291827, 0.6050312652222360477, 0.6586042779580459916, 0.7158509153455059337, 0.7781537217524819861, 0.8456603787764748192, 0.9191804452816982884, 1.000000000000000000 ),
 ( 0.000000000000000000, 1.000000000000000000 ),
 .UNSPECIFIED. ) ;
#17515 = LINE ( 'NONE', #9236, #5396 ) ;
#17516 = ORIENTED_EDGE ( 'NONE', *, *, #17856, .F. ) ;
#17517 = ORIENTED_EDGE ( 'NONE', *, *, #18055, .F. ) ;
#17518 = CARTESIAN_POINT ( 'NONE',  ( -7.922094096367543692, 41.68495194371154611, 78.88458188491442513 ) ) ;
#17519 = CARTESIAN_POINT ( 'NONE',  ( -4.699348147190207214, 37.07867987585471781, 75.97299512023676016 ) ) ;
#17520 = CARTESIAN_POINT ( 'NONE',  ( -7.308127660158699967, 41.72770130593617210, 76.16022115247204738 ) ) ;
#17521 = ORIENTED_EDGE ( 'NONE', *, *, #6981, .F. ) ;
#17522 = LINE ( 'NONE', #7847, #4333 ) ;
#17523 = CARTESIAN_POINT ( 'NONE',  ( -6.709785530345820703, 40.29707390701430825, 78.55233631870791555 ) ) ;
#17524 = CARTESIAN_POINT ( 'NONE',  ( -1.590937568396968871, 39.63064243629642647, 92.32933879953097289 ) ) ;
#17525 = EDGE_CURVE ( 'NONE', #16948, #6337, #1739, .T. ) ;
#17526 = ORIENTED_EDGE ( 'NONE', *, *, #17946, .T. ) ;
#17527 = DIRECTION ( 'NONE',  ( -1.402518428993831183E-16, 1.000000000000000000, -3.469446951953617640E-16 ) ) ;
#17528 = FILL_AREA_STYLE ('',( #14225 ) ) ;
#17529 = PLANE ( 'NONE',  #13254 ) ;
#17530 = CARTESIAN_POINT ( 'NONE',  ( 4.394343283833276992, 39.11584570990505938, 91.50808880123798872 ) ) ;
#17531 = CARTESIAN_POINT ( 'NONE',  ( 5.750640099535992533, 51.24052371918730842, 75.36022115247205022 ) ) ;
#17532 = B_SPLINE_CURVE_WITH_KNOTS ( 'NONE', 3,
 ( #5956, #7448, #13945, #12555, #4657, #6262, #17138, #17545, #5857, #6162, #11082 ),
 .UNSPECIFIED., .F., .F.,
 ( 4, 1, 1, 1, 1, 1, 1, 1, 4 ),
 ( 0.000000000000000000, 0.1891742793480645779, 0.3478164846204494509, 0.4767017694705349973, 0.5812052966572537338, 0.6755649002106222101, 0.7721207368275812000, 0.8786749842102796748, 1.000000000000000000 ),
 .UNSPECIFIED. ) ;
#17533 = DIRECTION ( 'NONE',  ( -0.5773502691896252870, 0.5773502691896259531, -0.5773502691896259531 ) ) ;
#17534 = CARTESIAN_POINT ( 'NONE',  ( 9.539487329945080418, 43.16218137147968292, 75.00433879953099847 ) ) ;
#17535 = CARTESIAN_POINT ( 'NONE',  ( -0.6601304159688821116, 52.21524791763957296, 79.16576412035692556 ) ) ;
#17536 = CARTESIAN_POINT ( 'NONE',  ( -4.195947902387222150, 37.45549797810746639, 76.06494828368110461 ) ) ;
#17537 = DIRECTION ( 'NONE',  ( 0.007885122365275663500, 0.9999689119394085113, 1.805443505845543142E-16 ) ) ;
#17538 = FACE_OUTER_BOUND ( 'NONE', #4428, .T. ) ;
#17539 = CARTESIAN_POINT ( 'NONE',  ( -0.9988176903691428077, 49.83852402762217082, 90.80496380123797451 ) ) ;
#17540 = ORIENTED_EDGE ( 'NONE', *, *, #6633, .F. ) ;
#17541 = CARTESIAN_POINT ( 'NONE',  ( 8.643837405878704416, 43.06427161293860451, 78.44945682776121032 ) ) ;
#17542 = CARTESIAN_POINT ( 'NONE',  ( -3.981178359372548492, 46.76218137147973408, 92.60183879953099506 ) ) ;
#17543 = CARTESIAN_POINT ( 'NONE',  ( 6.920970967149330910, 50.37604745108433946, 78.34373887323252461 ) ) ;
#17544 = DIRECTION ( 'NONE',  ( -0.5941461771851691553, -0.8043570849667760481, -2.357623395011396791E-16 ) ) ;
#17545 = CARTESIAN_POINT ( 'NONE',  ( 8.907015937602837496, 41.48861631773759484, 77.50814924735175282 ) ) ;
#17546 = CARTESIAN_POINT ( 'NONE',  ( 9.333517871656532350, 42.76686967087471913, 77.60952670463396430 ) ) ;
#17547 = DIRECTION ( 'NONE',  ( 0.000000000000000000, 2.168404344970984808E-15, -1.000000000000000000 ) ) ;
#17548 = CARTESIAN_POINT ( 'NONE',  ( 26.43948732994508788, 45.16218137147969003, 76.90433879953101837 ) ) ;
#17549 = CIRCLE ( 'NONE', #4282, 0.5999999999999928724 ) ;
#17550 = ORIENTED_EDGE ( 'NONE', *, *, #8959, .T. ) ;
#17551 = CARTESIAN_POINT ( 'NONE',  ( 8.851169967151879092, 41.32124240149376249, 78.93505401271374922 ) ) ;
#17552 = EDGE_CURVE ( 'NONE', #11899, #502, #2837, .T. ) ;
#17553 = CARTESIAN_POINT ( 'NONE',  ( 0.8455950101471346736, 52.35579997042385259, 78.52566232894263010 ) ) ;
#17554 = EDGE_CURVE ( 'NONE', #13579, #14654, #19584, .T. ) ;
#17555 = CARTESIAN_POINT ( 'NONE',  ( -7.611372734017126440, 43.12018948500615778, 78.28007409364852265 ) ) ;
#17556 = ORIENTED_EDGE ( 'NONE', *, *, #11962, .F. ) ;
#17557 = CARTESIAN_POINT ( 'NONE',  ( 1.250118884985844447, 46.34393909133126499, 80.45433879953087342 ) ) ;
#17558 = ADVANCED_FACE ( 'NONE', ( #8325 ), #14803, .T. ) ;
#17559 = B_SPLINE_CURVE_WITH_KNOTS ( 'NONE', 3,
 ( #20019, #885, #13446, #11856, #20342, #18652, #12070, #2492, #15258, #13657, #5781, #7371, #12286, #5454, #18765, #18334 ),
 .UNSPECIFIED., .F., .F.,
 ( 4, 2, 2, 2, 2, 2, 2, 4 ),
 ( 0.000000000000000000, 0.0007158805460618166512, 0.001431761092123633302, 0.001789701365154541682, 0.002147641638185449845, 0.002505581911216358225, 0.002684552047731790080, 0.002863522184247221502 ),
 .UNSPECIFIED. ) ;
#17560 = EDGE_CURVE ( 'NONE', #4848, #3564, #10251, .T. ) ;
#17561 = CARTESIAN_POINT ( 'NONE',  ( 5.544968037009670780, 45.50804040601273925, 91.19558880294498238 ) ) ;
#17562 = ORIENTED_EDGE ( 'NONE', *, *, #7826, .T. ) ;
#17563 = CARTESIAN_POINT ( 'NONE',  ( 5.848951923618479931, 37.15274410921379911, 76.58742703482498371 ) ) ;
#17564 = CARTESIAN_POINT ( 'NONE',  ( -0.9115598319063860089, 52.97844600157573325, 76.23506554152810111 ) ) ;
#17565 = CIRCLE ( 'NONE', #228, 15.24899959967967611 ) ;
#17566 = CARTESIAN_POINT ( 'NONE',  ( -4.385945807438902833, 50.73113084894660574, 76.01479905091014189 ) ) ;
#17567 = CARTESIAN_POINT ( 'NONE',  ( 5.939900590116411472, 51.10072461867315496, 76.90580938776616904 ) ) ;
#17568 = SURFACE_STYLE_USAGE ( .BOTH. , #17259 ) ;
#17569 = CARTESIAN_POINT ( 'NONE',  ( 2.841819011512540794, 48.97028086682659875, 92.45433879953095868 ) ) ;
#17570 = EDGE_LOOP ( 'NONE', ( #12827, #5236, #17149, #12637 ) ) ;
#17571 = CARTESIAN_POINT ( 'NONE',  ( 8.896031707678503153, 41.45569588382780779, 75.98771331677210128 ) ) ;
#17572 = ORIENTED_EDGE ( 'NONE', *, *, #5168, .F. ) ;
#17573 = FACE_OUTER_BOUND ( 'NONE', #1010, .T. ) ;
#17574 = CARTESIAN_POINT ( 'NONE',  ( -0.9988176903691428077, 49.83852402762217082, 95.64871380123798872 ) ) ;
#17575 = PLANE ( 'NONE',  #18974 ) ;
#17576 = CARTESIAN_POINT ( 'NONE',  ( 5.845446004764687231, 37.15023890796076245, 76.33129752952908120 ) ) ;
#17577 = CARTESIAN_POINT ( 'NONE',  ( -7.306329150795409788, 41.74985974580818748, 78.93438826577718714 ) ) ;
#17578 = CIRCLE ( 'NONE', #18604, 8.199999999999995737 ) ;
#17579 = ORIENTED_EDGE ( 'NONE', *, *, #1930, .T. ) ;
#17580 = CARTESIAN_POINT ( 'NONE',  ( 4.577379499810326990, 52.10716406238486087, 78.43496551412393103 ) ) ;
#17581 = ORIENTED_EDGE ( 'NONE', *, *, #6139, .T. ) ;
#17582 = CARTESIAN_POINT ( 'NONE',  ( -3.269139879056130571, 51.34905839445515596, 75.61719165653033770 ) ) ;
#17583 = EDGE_CURVE ( 'NONE', #8220, #4311, #8748, .T. ) ;
#17584 = CARTESIAN_POINT ( 'NONE',  ( -5.154188915835984375, 42.64120994080404614, 92.36746380123797451 ) ) ;
#17585 = CARTESIAN_POINT ( 'NONE',  ( 4.776132423410367700, 51.96035328397762498, 75.67068799376596644 ) ) ;
#17586 = ORIENTED_EDGE ( 'NONE', *, *, #16583, .T. ) ;
#17587 = CARTESIAN_POINT ( 'NONE',  ( -5.384655767683054428, 49.83721677713893428, 78.57924047249254329 ) ) ;
#17588 = CARTESIAN_POINT ( 'NONE',  ( 5.928963754087450688, 43.92611494815086814, 93.65746379611699979 ) ) ;
#17589 = AXIS2_PLACEMENT_3D ( 'NONE', #15124, #3833, #8740 ) ;
#17590 = CARTESIAN_POINT ( 'NONE',  ( 4.410764955181007529, 36.12506835695402430, 76.35980278528342069 ) ) ;
#17591 = CARTESIAN_POINT ( 'NONE',  ( 5.724311780639353309, 51.25997138778688367, 75.97249762499970416 ) ) ;
#17592 = DIRECTION ( 'NONE',  ( 3.893792155548169402E-16, 7.183611964723547524E-17, -1.000000000000000000 ) ) ;
#17593 = ORIENTED_EDGE ( 'NONE', *, *, #1080, .T. ) ;
#17594 = CARTESIAN_POINT ( 'NONE',  ( -4.913882109623730621, 44.60549673912475299, 92.55433879953093879 ) ) ;
#17595 = CARTESIAN_POINT ( 'NONE',  ( 6.828503391016846891, 43.33193468930419101, 92.91433880123798872 ) ) ;
#17596 = ORIENTED_EDGE ( 'NONE', *, *, #19482, .T. ) ;
#17597 = CARTESIAN_POINT ( 'NONE',  ( 4.140865811708774658, 51.51558413471341424, 78.38317481739672132 ) ) ;
#17598 = CARTESIAN_POINT ( 'NONE',  ( 0.5221537403065181771, 44.16218137147969003, 56.15433879953099705 ) ) ;
#17599 = CARTESIAN_POINT ( 'NONE',  ( 0.8308482478495438084, 52.95678316823124732, 78.75697940203460234 ) ) ;
#17600 = CARTESIAN_POINT ( 'NONE',  ( -1.419351766502868761, 49.49642391118513274, 94.90746379782397923 ) ) ;
#17601 = CARTESIAN_POINT ( 'NONE',  ( 4.522153740306500858, 44.16218137147969003, 105.5543387995310098 ) ) ;
#17602 = LINE ( 'NONE', #17714, #20013 ) ;
#17603 = AXIS2_PLACEMENT_3D ( 'NONE', #4941, #1975, #5152 ) ;
#17604 = FACE_OUTER_BOUND ( 'NONE', #2400, .T. ) ;
#17605 = ORIENTED_EDGE ( 'NONE', *, *, #10682, .T. ) ;
#17606 = CARTESIAN_POINT ( 'NONE',  ( -7.099600269029870958, 47.18725423407072128, 78.26805218182843760 ) ) ;
#17607 = CARTESIAN_POINT ( 'NONE',  ( 5.760694563098077481, 51.23309689197249384, 79.54845644658969661 ) ) ;
#17608 = ORIENTED_EDGE ( 'NONE', *, *, #11160, .F. ) ;
#17609 = CARTESIAN_POINT ( 'NONE',  ( -7.802862648839750115, 41.30999248941007806, 78.30232473790640313 ) ) ;
#17610 = LINE ( 'NONE', #6322, #5494 ) ;
#17611 = CARTESIAN_POINT ( 'NONE',  ( 9.244427017087200937, 42.49985872791199881, 79.25343573416346032 ) ) ;
#17612 = ORIENTED_EDGE ( 'NONE', *, *, #11811, .T. ) ;
#17613 = DIRECTION ( 'NONE',  ( 1.540237394707283727E-16, 1.793354297423763257E-16, -1.000000000000000000 ) ) ;
#17614 = ORIENTED_EDGE ( 'NONE', *, *, #1581, .F. ) ;
#17615 = CARTESIAN_POINT ( 'NONE',  ( -4.274404157479777311, 37.68962381543027362, 75.36022115247205022 ) ) ;
#17616 = CARTESIAN_POINT ( 'NONE',  ( -1.219056181836354558, 49.77488197367695477, 93.31237966814926210 ) ) ;
#17617 = CARTESIAN_POINT ( 'NONE',  ( -7.042421365581803983, 40.99363011463105977, 77.06266651728316219 ) ) ;
#17618 = EDGE_LOOP ( 'NONE', ( #731, #18687, #4185, #9992, #17275, #8839, #4969, #5990 ) ) ;
#17619 = CARTESIAN_POINT ( 'NONE',  ( 4.577225057937401864, 52.10727814237509392, 78.46169174070733732 ) ) ;
#17620 = CARTESIAN_POINT ( 'NONE',  ( -4.790295051490115696, 37.92061980927154963, 77.90139762306027649 ) ) ;
#17621 = CARTESIAN_POINT ( 'NONE',  ( -4.007890887056448470, 40.01116025973682611, 91.39183879782399345 ) ) ;
#17622 = VECTOR ( 'NONE', #5580, 1000.000000000000114 ) ;
#17623 = ORIENTED_EDGE ( 'NONE', *, *, #18748, .F. ) ;
#17624 = CARTESIAN_POINT ( 'NONE',  ( 8.617838889373357958, 45.46597658821364263, 78.74919174070734584 ) ) ;
#17625 = CARTESIAN_POINT ( 'NONE',  ( 0.5221537403065010796, 44.16218137147969003, 95.05433879953098142 ) ) ;
#17626 = CARTESIAN_POINT ( 'NONE',  ( 5.939900590116411472, 51.10072461867315496, 76.38301527011910252 ) ) ;
#17627 = CARTESIAN_POINT ( 'NONE',  ( 2.043125170982144745, 38.48583871533720213, 92.67996380123798872 ) ) ;
#17628 = EDGE_CURVE ( 'NONE', #14506, #4469, #15275, .T. ) ;
#17629 = CARTESIAN_POINT ( 'NONE',  ( 6.319761386105714251, 38.36299381901618233, 78.05707163992254038 ) ) ;
#17630 = CARTESIAN_POINT ( 'NONE',  ( 0.5283203121033563932, 52.96651480206464413, 76.89772265631788173 ) ) ;
#17631 = CARTESIAN_POINT ( 'NONE',  ( -0.7268458593731683681, 40.36218137147969998, 46.35433879953098568 ) ) ;
#17632 = VECTOR ( 'NONE', #10021, 999.9999999999998863 ) ;
#17633 = CARTESIAN_POINT ( 'NONE',  ( -0.4245371128412744888, 52.21339017786244341, 79.34012451928875009 ) ) ;
#17634 = ORIENTED_EDGE ( 'NONE', *, *, #18874, .T. ) ;
#17635 = DIRECTION ( 'NONE',  ( -0.000000000000000000, -0.000000000000000000, 1.000000000000000000 ) ) ;
#17636 = CARTESIAN_POINT ( 'NONE',  ( 4.199109002476567376, 47.83913663364971569, 93.48786078214052964 ) ) ;
#17637 = CARTESIAN_POINT ( 'NONE',  ( 8.579956030688345336, 40.50839702842124268, 79.37958223971880045 ) ) ;
#17638 = CARTESIAN_POINT ( 'NONE',  ( 6.923000991621626632, 50.37454795378102546, 78.43783143115764744 ) ) ;
#17639 = ORIENTED_EDGE ( 'NONE', *, *, #9153, .T. ) ;
#17640 = AXIS2_PLACEMENT_3D ( 'NONE', #3558, #11556, #16336 ) ;
#17641 = ORIENTED_EDGE ( 'NONE', *, *, #14561, .F. ) ;
#17642 = VECTOR ( 'NONE', #10179, 1000.000000000000000 ) ;
#17643 = CARTESIAN_POINT ( 'NONE',  ( 7.887664428531886429, 40.55654679518931260, 75.60913502469634295 ) ) ;
#17644 = DIRECTION ( 'NONE',  ( 0.9539696396349547358, -0.2999031954727301441, 9.315070279690498823E-17 ) ) ;
#17645 = FACE_OUTER_BOUND ( 'NONE', #7136, .T. ) ;
#17646 = DIRECTION ( 'NONE',  ( -1.000000000000000000, 1.110223024625156540E-16, -1.779391786395883043E-16 ) ) ;
#17647 = DIRECTION ( 'NONE',  ( -1.000000000000000000, 0.000000000000000000, 0.000000000000000000 ) ) ;
#17648 = VECTOR ( 'NONE', #20715, 1000.000000000000000 ) ;
#17649 = EDGE_CURVE ( 'NONE', #3704, #13088, #13522, .T. ) ;
#17650 = PLANE ( 'NONE',  #5668 ) ;
#17651 = CARTESIAN_POINT ( 'NONE',  ( 8.643936145691096584, 43.06456754242027074, 77.06316232894263862 ) ) ;
#17652 = CARTESIAN_POINT ( 'NONE',  ( 31.07218010054375412, 42.96218137147968008, 69.40574467885102194 ) ) ;
#17653 = AXIS2_PLACEMENT_3D ( 'NONE', #595, #7077, #10517 ) ;
#17654 = VECTOR ( 'NONE', #17117, 1000.000000000000000 ) ;
#17655 = CARTESIAN_POINT ( 'NONE',  ( -4.859530362865112529, 37.19700002604054134, 79.54807357191100436 ) ) ;
#17656 = EDGE_CURVE ( 'NONE', #15461, #14881, #20210, .T. ) ;
#17657 = CARTESIAN_POINT ( 'NONE',  ( 27.03948732994508930, 43.16218137147969003, 76.90433879953101837 ) ) ;
#17658 = CARTESIAN_POINT ( 'NONE',  ( 5.410058914415630582, 36.83912723373610731, 78.11840496518735222 ) ) ;
#17659 = AXIS2_PLACEMENT_3D ( 'NONE', #8907, #16772, #3986 ) ;
#17660 = VECTOR ( 'NONE', #11560, 1000.000000000000114 ) ;
#17661 = EDGE_CURVE ( 'NONE', #7199, #13044, #3731, .T. ) ;
#17662 = ORIENTED_EDGE ( 'NONE', *, *, #3112, .T. ) ;
#17663 = CARTESIAN_POINT ( 'NONE',  ( -4.477846259693498254, 37.66218137147969713, 53.35433879953099989 ) ) ;
#17664 = CARTESIAN_POINT ( 'NONE',  ( 8.386307069575464013, 39.92801880710491957, 76.83374382764255017 ) ) ;
#17665 = ORIENTED_EDGE ( 'NONE', *, *, #10455, .T. ) ;
#17667 = VECTOR ( 'NONE', #2798, 1000.000000000000000 ) ;
#17666 = CARTESIAN_POINT ( 'NONE',  ( 6.386300776676741897, 37.53671392601205525, 75.49608936836499140 ) ) ;
#17668 = CARTESIAN_POINT ( 'NONE',  ( 8.879174460483845621, 41.40517364458161609, 78.05744560429982926 ) ) ;
#17669 = DIRECTION ( 'NONE',  ( 1.779391786395883536E-16, 5.922860397471806844E-17, -1.000000000000000000 ) ) ;
#17670 = CARTESIAN_POINT ( 'NONE',  ( 0.6753953261465888147, 52.35350465892279459, 75.98308111960244560 ) ) ;
#17671 = DIRECTION ( 'NONE',  ( 0.9999689119394086223, -0.007885122365275665235, 1.526048693634353392E-16 ) ) ;
#17672 = EDGE_CURVE ( 'NONE', #17850, #12203, #18529, .T. ) ;
#17673 = EDGE_LOOP ( 'NONE', ( #3567, #1401, #8905, #2915 ) ) ;
#17674 = EDGE_CURVE ( 'NONE', #18944, #15539, #3840, .T. ) ;
#17675 = FACE_OUTER_BOUND ( 'NONE', #13541, .T. ) ;
#17676 = EDGE_CURVE ( 'NONE', #970, #8464, #18741, .T. ) ;
#17677 = EDGE_LOOP ( 'NONE', ( #7679, #9910, #12770, #1786 ) ) ;
#17678 = LINE ( 'NONE', #1306, #10134 ) ;
#17679 =( GEOMETRIC_REPRESENTATION_CONTEXT ( 3 ) GLOBAL_UNCERTAINTY_ASSIGNED_CONTEXT ( ( #12954 ) ) GLOBAL_UNIT_ASSIGNED_CONTEXT ( ( #6145, #14547, #7957 ) ) REPRESENTATION_CONTEXT ( 'NONE', 'WORKASPACE' ) );
#17680 = CARTESIAN_POINT ( 'NONE',  ( 2.043125170982144745, 38.48583871533720213, 93.77371380123798872 ) ) ;
#17681 = CARTESIAN_POINT ( 'NONE',  ( 0.3869120917952209582, 35.96329670974013482, 78.57639762306027365 ) ) ;
#17682 = PRODUCT_DEFINITION ( 'UNKNOWN', '', #32, #852 ) ;
#17683 = B_SPLINE_CURVE_WITH_KNOTS ( 'NONE', 3,
 ( #13484, #19955, #12111, #5607, #5504, #1900, #10099, #11700, #6782, #10320, #8810, #16479, #20069, #290, #16581, #3591, #16793, #503, #14985 ),
 .UNSPECIFIED., .F., .F.,
 ( 4, 1, 1, 1, 1, 1, 1, 1, 1, 1, 1, 1, 1, 1, 1, 1, 4 ),
 ( 0.000000000000000000, 0.05434379794353864229, 0.1062390698768248820, 0.1553778989748225425, 0.2029887854916514467, 0.2486500052201169320, 0.2921085583616858661, 0.3352193261980264682, 0.3771870632897987852, 0.4223876994541358454, 0.4752030700363142346, 0.5373302487560115415, 0.6091097927081512431, 0.6911313100281405442, 0.7836801803933998167, 0.8864064767870927231, 1.000000000000000000 ),
 .UNSPECIFIED. ) ;
#17684 = FACE_OUTER_BOUND ( 'NONE', #8125, .T. ) ;
#17685 = DIRECTION ( 'NONE',  ( 3.154042683594179047E-15, 4.423602989573997160E-31, -1.000000000000000000 ) ) ;
#17686 = EDGE_CURVE ( 'NONE', #4618, #11143, #6627, .T. ) ;
#17687 = B_SPLINE_SURFACE_WITH_KNOTS ( 'NONE', 3, 1, ( 
 ( #5103, #18095 ),
 ( #16186, #11621 ),
 ( #19571, #19470 ),
 ( #1612, #11408 ),
 ( #17985, #4887 ),
 ( #8414, #12994 ),
 ( #11306, #9920 ),
 ( #16405, #1827 ),
 ( #3301, #8312 ),
 ( #20612, #11064 ),
 ( #12751, #6149 ),
 ( #17435, #4549 ),
 ( #17633, #3178 ),
 ( #9680, #15949 ),
 ( #7859, #6251 ),
 ( #3069, #1370 ),
 ( #17535, #14348 ),
 ( #4644, #12851 ),
 ( #8062, #1478 ),
 ( #21019, #9571 ),
 ( #20822, #19228 ),
 ( #11165, #2956 ),
 ( #14232, #14554 ),
 ( #18920, #4336 ),
 ( #16056, #2859 ),
 ( #20915, #12543 ),
 ( #19031, #7964 ),
 ( #14449, #17748 ),
 ( #9464, #10862 ),
 ( #1260, #17332 ),
 ( #6348, #7753 ) ),
 .UNSPECIFIED., .F., .F., .F.,
 ( 4, 1, 1, 1, 1, 1, 1, 1, 1, 1, 1, 1, 1, 1, 1, 1, 1, 1, 1, 1, 1, 1, 1, 1, 1, 1, 1, 1, 4 ),
 ( 2, 2 ),
 ( 0.000000000000000000, 0.04384681544484739235, 0.08567827314907716652, 0.1254967717429318341, 0.1636614238475955219, 0.1996619864010514556, 0.2341576300211750672, 0.2670604349552898049, 0.2981387414117787626, 0.3278414694467580159, 0.3565940729939165998, 0.3842752990321527395, 0.4112124433481792463, 0.4371802474119553250, 0.4623137086418128150, 0.4873144965356236424, 0.5115863199873472711, 0.5585256650453194194, 0.6022882070645410035, 0.6442466772295868394, 0.6853175287114940950, 0.7081315191531365461, 0.7355471538020152966, 0.7678357380769914586, 0.8047386325758049130, 0.8465390724922580157, 0.8929683470010029156, 0.9440341083467609362, 1.000000000000000000 ),
 ( 0.000000000000000000, 1.000000000000000000 ),
 .UNSPECIFIED. ) ;
#17688 = AXIS2_PLACEMENT_3D ( 'NONE', #951, #18402, #16911 ) ;
#17689 = VERTEX_POINT ( 'NONE', #20633 ) ;
#17690 = PLANE ( 'NONE',  #7097 ) ;
#17691 = ORIENTED_EDGE ( 'NONE', *, *, #20735, .F. ) ;
#17692 = CARTESIAN_POINT ( 'NONE',  ( -3.358136819263964234, 52.20524002164697208, 76.41354228756682687 ) ) ;
#17693 = CARTESIAN_POINT ( 'NONE',  ( -7.890048607039471307, 46.74575480130646099, 79.45433879953087342 ) ) ;
#17694 = CARTESIAN_POINT ( 'NONE',  ( 4.544296722651392173, 52.13160097721661401, 76.36737811492949390 ) ) ;
#17695 = ORIENTED_EDGE ( 'NONE', *, *, #11988, .T. ) ;
#17696 = CARTESIAN_POINT ( 'NONE',  ( 6.635267586053947397, 39.64667042487232607, 72.45432679953087529 ) ) ;
#17697 = CYLINDRICAL_SURFACE ( 'NONE', #5525, 6.000000000000001776 ) ;
#17698 = CARTESIAN_POINT ( 'NONE',  ( -4.588243132438925009, 36.99661107704093865, 78.89954634079194307 ) ) ;
#17699 = CARTESIAN_POINT ( 'NONE',  ( -4.073823749297678098, 50.94692091219555152, 78.85744209785094938 ) ) ;
#17700 = CARTESIAN_POINT ( 'NONE',  ( 5.442040249694054310, 36.86197992501465137, 77.64535406911728899 ) ) ;
#17701 = ORIENTED_EDGE ( 'NONE', *, *, #5060, .T. ) ;
#17702 = DIRECTION ( 'NONE',  ( -1.290716872006552287E-16, -1.000000000000000000, 0.000000000000000000 ) ) ;
#17703 = FACE_OUTER_BOUND ( 'NONE', #1655, .T. ) ;
#17704 = ORIENTED_EDGE ( 'NONE', *, *, #19506, .T. ) ;
#17705 = CARTESIAN_POINT ( 'NONE',  ( 4.661266133293011649, 52.04520038539091331, 77.98100106196224601 ) ) ;
#17706 = DIRECTION ( 'NONE',  ( 3.893792155548169402E-16, 7.183611964723547524E-17, -1.000000000000000000 ) ) ;
#17707 = EDGE_CURVE ( 'NONE', #13088, #2032, #11088, .T. ) ;
#17708 = DIRECTION ( 'NONE',  ( -1.540237394707284220E-16, -1.793354297423764243E-16, 1.000000000000000000 ) ) ;
#17709 = CARTESIAN_POINT ( 'NONE',  ( 0.5886017282102210535, 52.96193049659134999, 78.93669174070734584 ) ) ;
#17710 = CARTESIAN_POINT ( 'NONE',  ( 6.660594192354429843, 43.89417127335556046, 92.01683879782399345 ) ) ;
#17711 = CARTESIAN_POINT ( 'NONE',  ( -1.876873622437039257, 39.01745058958429269, 92.71996379782397923 ) ) ;
#17712 = EDGE_CURVE ( 'NONE', #13044, #16046, #10946, .T. ) ;
#17713 = VECTOR ( 'NONE', #10168, 1000.000000000000227 ) ;
#17714 = CARTESIAN_POINT ( 'NONE',  ( 2.029186242314200861, 35.35002428291939225, 76.86610350541323555 ) ) ;
#17715 = ADVANCED_FACE ( 'NONE', ( #12772 ), #15773, .T. ) ;
#17716 = CARTESIAN_POINT ( 'NONE',  ( 5.939900590116411472, 51.10072461867315496, 76.38301527011910252 ) ) ;
#17717 = VERTEX_POINT ( 'NONE', #4356 ) ;
#17718 = CARTESIAN_POINT ( 'NONE',  ( 1.984707218798539730, 52.83985775011834107, 77.14939308509356408 ) ) ;
#17719 = ORIENTED_EDGE ( 'NONE', *, *, #947, .F. ) ;
#17720 = DIRECTION ( 'NONE',  ( -0.3330135628418914862, -0.9429220365244147528, -2.203913228770411492E-16 ) ) ;
#17721 = CARTESIAN_POINT ( 'NONE',  ( 8.214799251806553571, 41.32260305165857517, 72.45433879953087342 ) ) ;
#17722 = CARTESIAN_POINT ( 'NONE',  ( 8.949781629519392823, 41.61678780941641520, 75.36311794487049553 ) ) ;
#17723 = ORIENTED_EDGE ( 'NONE', *, *, #9534, .T. ) ;
#17724 = CARTESIAN_POINT ( 'NONE',  ( 8.385679600361122255, 39.92613824206362949, 77.13595644658970230 ) ) ;
#17725 = ORIENTED_EDGE ( 'NONE', *, *, #10377, .F. ) ;
#17726 = VECTOR ( 'NONE', #1658, 1000.000000000000000 ) ;
#17727 = CARTESIAN_POINT ( 'NONE',  ( -7.881634263515648442, 41.55089060731901185, 78.93495394624521566 ) ) ;
#17728 = CARTESIAN_POINT ( 'NONE',  ( -4.525716193177020230, 36.95042494574692427, 76.22840587216694530 ) ) ;
#17729 = FACE_OUTER_BOUND ( 'NONE', #7953, .T. ) ;
#17730 = VECTOR ( 'NONE', #20799, 1000.000000000000000 ) ;
#17731 = VERTEX_POINT ( 'NONE', #6062 ) ;
#17732 = CARTESIAN_POINT ( 'NONE',  ( -5.087398782055177371, 37.36531724819641198, 77.33565342272370913 ) ) ;
#17733 = CARTESIAN_POINT ( 'NONE',  ( -7.313565574299385474, 41.74526126053015673, 79.54845644658969661 ) ) ;
#17734 = CARTESIAN_POINT ( 'NONE',  ( 5.856396280011940902, 46.10368687828906076, 91.93871379782397923 ) ) ;
#17735 = ORIENTED_EDGE ( 'NONE', *, *, #4760, .F. ) ;
#17736 = CARTESIAN_POINT ( 'NONE',  ( -7.788095026490401196, 41.26728263494260318, 78.81763427810251699 ) ) ;
#17737 = CARTESIAN_POINT ( 'NONE',  ( 5.544276951911416340, 50.64433212932689088, 78.59183879953087626 ) ) ;
#17738 = DIRECTION ( 'NONE',  ( -6.079324319404144630E-32, 3.469446951953617147E-16, 1.000000000000000000 ) ) ;
#17739 = CARTESIAN_POINT ( 'NONE',  ( -5.154188915835984375, 42.64120994080404614, 91.11746380123797451 ) ) ;
#17740 =( NAMED_UNIT ( * ) SI_UNIT ( $, .STERADIAN. ) SOLID_ANGLE_UNIT ( ) );
#17741 = CARTESIAN_POINT ( 'NONE',  ( -4.924280525269182363, 51.08613106951644767, 75.37785507730471579 ) ) ;
#17742 = CARTESIAN_POINT ( 'NONE',  ( -4.361665858399769391, 37.57520132541210245, 75.97198585835440099 ) ) ;
#17743 = VECTOR ( 'NONE', #17433, 1000.000000000000000 ) ;
#17744 = FACE_OUTER_BOUND ( 'NONE', #3525, .T. ) ;
#17745 = ORIENTED_EDGE ( 'NONE', *, *, #18621, .F. ) ;
#17746 = DIRECTION ( 'NONE',  ( 1.084202172485505420E-16, 1.000000000000000000, 0.000000000000000000 ) ) ;
#17747 = VECTOR ( 'NONE', #10872, 1000.000000000000000 ) ;
#17748 = CARTESIAN_POINT ( 'NONE',  ( -0.9366413518729753696, 52.97986903894317834, 78.07640427701528552 ) ) ;
#17749 = ORIENTED_EDGE ( 'NONE', *, *, #6651, .T. ) ;
#17750 = FACE_OUTER_BOUND ( 'NONE', #15435, .T. ) ;
#17751 = CARTESIAN_POINT ( 'NONE',  ( -1.535769738210056579, 49.45816841730323432, 94.29858131124046849 ) ) ;
#17752 = CARTESIAN_POINT ( 'NONE',  ( 8.414968994577074923, 40.01392041461337357, 78.89537297773202340 ) ) ;
#17753 = CARTESIAN_POINT ( 'NONE',  ( 6.873747143562635387, 50.41092978727617435, 78.08828162113617566 ) ) ;
#17754 = ORIENTED_EDGE ( 'NONE', *, *, #4634, .F. ) ;
#17755 = ORIENTED_EDGE ( 'NONE', *, *, #178, .F. ) ;
#17756 = VECTOR ( 'NONE', #4290, 1000.000000000000114 ) ;
#17757 = CARTESIAN_POINT ( 'NONE',  ( 0.5221537403065019678, 44.16218137147968292, 72.45433879953087342 ) ) ;
#17758 = PRESENTATION_STYLE_ASSIGNMENT (( #17858 ) ) ;
#17759 = CARTESIAN_POINT ( 'NONE',  ( -4.889784912074394363, 37.21934784281386044, 78.69750623079058016 ) ) ;
#17760 = DIRECTION ( 'NONE',  ( -1.000000000000000000, -4.924280921909907046E-16, -5.626130192357177659E-16 ) ) ;
#17761 = CIRCLE ( 'NONE', #20476, 4.200000000000003730 ) ;
#17762 = PLANE ( 'NONE',  #14731 ) ;
#17763 = DIRECTION ( 'NONE',  ( 0.000000000000000000, 0.000000000000000000, 1.000000000000000000 ) ) ;
#17764 = LINE ( 'NONE', #10702, #1261 ) ;
#17765 = CARTESIAN_POINT ( 'NONE',  ( 6.519277697500823976, 49.74792914119518628, 76.69700829373513784 ) ) ;
#17766 = CARTESIAN_POINT ( 'NONE',  ( -7.677846259693484221, 47.36218137147966445, 53.35433879953099989 ) ) ;
#17767 = LINE ( 'NONE', #8910, #18469 ) ;
#17768 = ORIENTED_EDGE ( 'NONE', *, *, #4693, .T. ) ;
#17769 = CARTESIAN_POINT ( 'NONE',  ( -5.159531558744112623, 38.35460532074419859, 79.39214668191834789 ) ) ;
#17770 = AXIS2_PLACEMENT_3D ( 'NONE', #5819, #11048, #12325 ) ;
#17771 = CARTESIAN_POINT ( 'NONE',  ( 0.5221537403065105165, 40.96218137147968719, 45.55433879953100273 ) ) ;
#17772 = EDGE_CURVE ( 'NONE', #19487, #6017, #8208, .T. ) ;
#17773 = CARTESIAN_POINT ( 'NONE',  ( 5.270142054182215041, 50.84773347817210265, 78.86068376280545067 ) ) ;
#17774 = CARTESIAN_POINT ( 'NONE',  ( 0.5221537403065019678, 51.36218137147968577, 83.03825919817350609 ) ) ;
#17775 = CARTESIAN_POINT ( 'NONE',  ( 8.491906929791015912, 40.24450828730113727, 75.69429397690826988 ) ) ;
#17776 = EDGE_LOOP ( 'NONE', ( #1340, #6121, #18412, #4802 ) ) ;
#17777 = CARTESIAN_POINT ( 'NONE',  ( 6.877103025211564358, 37.88742324339783352, 76.41040896618429201 ) ) ;
#17778 = DIRECTION ( 'NONE',  ( 0.3165065846431828200, 0.9485903129789527988, 0.000000000000000000 ) ) ;
#17779 = CARTESIAN_POINT ( 'NONE',  ( 6.467096401101858127, 37.59444752110963606, 78.28436300994860630 ) ) ;
#17780 = DIRECTION ( 'NONE',  ( -0.9534635866061451637, -0.3015081906286225522, -2.009271279954815797E-16 ) ) ;
#17781 = DIRECTION ( 'NONE',  ( -0.9485903129789527988, 0.3165065846431829311, -8.934458285744989980E-17 ) ) ;
#17782 = ORIENTED_EDGE ( 'NONE', *, *, #19537, .T. ) ;
#17783 = CARTESIAN_POINT ( 'NONE',  ( 8.951454296033540814, 41.62180089707131003, 76.31823237213514233 ) ) ;
#17784 = VECTOR ( 'NONE', #20725, 1000.000000000000000 ) ;
#17785 = EDGE_CURVE ( 'NONE', #10020, #13175, #9440, .T. ) ;
#17786 = ORIENTED_EDGE ( 'NONE', *, *, #2997, .F. ) ;
#17787 = CARTESIAN_POINT ( 'NONE',  ( -2.416137431568557314, 39.07291177436112406, 92.36746380123797451 ) ) ;
#17788 = CARTESIAN_POINT ( 'NONE',  ( -0.9988176903691428077, 49.83852402762217082, 94.39871380123798872 ) ) ;
#17789 = CARTESIAN_POINT ( 'NONE',  ( -7.861899879695211091, 46.83617027511139241, 79.36034011475112493 ) ) ;
#17790 = LINE ( 'NONE', #19378, #18486 ) ;
#17791 = CARTESIAN_POINT ( 'NONE',  ( 23.03948732994508575, 43.16218137147969003, 73.00433879953099847 ) ) ;
#17792 = ADVANCED_FACE ( 'NONE', ( #15972 ), #7774, .T. ) ;
#17793 = VERTEX_POINT ( 'NONE', #9173 ) ;
#17794 = DIRECTION ( 'NONE',  ( -0.000000000000000000, -0.000000000000000000, 1.000000000000000000 ) ) ;
#17795 = ORIENTED_EDGE ( 'NONE', *, *, #287, .T. ) ;
#17796 = VECTOR ( 'NONE', #9090, 1000.000000000000227 ) ;
#17797 = CARTESIAN_POINT ( 'NONE',  ( -2.938357031425011812, 51.58542370663933241, 76.25796290525131838 ) ) ;
#17798 = CARTESIAN_POINT ( 'NONE',  ( 5.568489401881125289, 48.03437091500646261, 91.82058880123797451 ) ) ;
#17799 = EDGE_LOOP ( 'NONE', ( #4702, #11904, #3436, #8007, #3248, #3281, #19890, #14213, #9727, #4509, #6107, #1740 ) ) ;
#17800 = EDGE_CURVE ( 'NONE', #17463, #7261, #15868, .T. ) ;
#17801 = DIRECTION ( 'NONE',  ( 0.000000000000000000, 0.000000000000000000, 1.000000000000000000 ) ) ;
#17802 = CARTESIAN_POINT ( 'NONE',  ( 11.22215374030649926, 39.96218137147969429, 80.55433879953099563 ) ) ;
#17803 = CARTESIAN_POINT ( 'NONE',  ( 5.691650701599316520, 41.94760153193540475, 92.55433879953103826 ) ) ;
#17804 = DIRECTION ( 'NONE',  ( 0.3165065846431826535, 0.9485903129789529098, 2.188653791613874008E-16 ) ) ;
#17805 = DIRECTION ( 'NONE',  ( -0.3165065846431826535, -0.9485903129789529098, -2.188653791613874008E-16 ) ) ;
#17806 = ORIENTED_EDGE ( 'NONE', *, *, #17369, .F. ) ;
#17807 = CARTESIAN_POINT ( 'NONE',  ( 2.029186242314200861, 35.35002428291939225, 76.86610350541323555 ) ) ;
#17808 = CARTESIAN_POINT ( 'NONE',  ( 0.8501571860830551275, 52.96349708516230237, 78.54797669815580718 ) ) ;
#17809 = ORIENTED_EDGE ( 'NONE', *, *, #4818, .T. ) ;
#17810 = CARTESIAN_POINT ( 'NONE',  ( 4.577678780824717464, 52.10694299555530051, 78.38317481739672132 ) ) ;
#17811 = PLANE ( 'NONE',  #4330 ) ;
#17812 = CARTESIAN_POINT ( 'NONE',  ( -5.483735557913453462, 50.68636498614493036, 75.61447646545406087 ) ) ;
#17813 = CARTESIAN_POINT ( 'NONE',  ( -3.134114116279073770, 48.15229756555780227, 95.37621379611701400 ) ) ;
#17814 = CARTESIAN_POINT ( 'NONE',  ( 5.052198367669454626, 48.31320248322254685, 93.26683879782399345 ) ) ;
#17815 = LINE ( 'NONE', #52, #13917 ) ;
#17816 = ORIENTED_EDGE ( 'NONE', *, *, #4198, .T. ) ;
#17817 = CARTESIAN_POINT ( 'NONE',  ( 1.853273245406973135, 52.20358242324970632, 79.18222496875146987 ) ) ;
#17818 = EDGE_CURVE ( 'NONE', #4298, #12829, #2777, .T. ) ;
#17819 = ORIENTED_EDGE ( 'NONE', *, *, #5940, .F. ) ;
#17820 = DIRECTION ( 'NONE',  ( -1.334402673828316297E-16, 2.168404344970984413E-15, 1.000000000000000000 ) ) ;
#17821 = EDGE_CURVE ( 'NONE', #5789, #791, #3093, .T. ) ;
#17822 = DIRECTION ( 'NONE',  ( 0.000000000000000000, -1.000000000000000000, 2.168404344970984808E-15 ) ) ;
#17823 = CARTESIAN_POINT ( 'NONE',  ( 9.092498755203211047, 42.04452008889646208, 79.47377622490290605 ) ) ;
#17824 = VERTEX_POINT ( 'NONE', #15664 ) ;
#17825 = CARTESIAN_POINT ( 'NONE',  ( 5.599418364623888422, 51.35222512318382826, 78.27515171461519117 ) ) ;
#17826 = CARTESIAN_POINT ( 'NONE',  ( -5.810228987958478086, 37.89924280392040856, 75.80435357840198662 ) ) ;
#17827 = VERTEX_POINT ( 'NONE', #17354 ) ;
#17828 = CARTESIAN_POINT ( 'NONE',  ( 6.882736312352589536, 37.89144858414100270, 77.26022115247205591 ) ) ;
#17829 = CARTESIAN_POINT ( 'NONE',  ( 8.372294911086104463, 41.79245952794141772, 78.82125883816432577 ) ) ;
#17830 = ADVANCED_FACE ( 'NONE', ( #16078 ), #20430, .T. ) ;
#17831 = CARTESIAN_POINT ( 'NONE',  ( 6.102441102155617969, 43.42752260303680600, 95.80496379953099506 ) ) ;
#17832 = B_SPLINE_CURVE_WITH_KNOTS ( 'NONE', 3,
 ( #10959, #14228, #9676, #1577, #16256, #6037, #14550, #2855, #9774, #17629, #1256, #3063, #7749, #20707, #19133, #6146 ),
 .UNSPECIFIED., .F., .F.,
 ( 4, 2, 2, 2, 2, 2, 2, 4 ),
 ( 0.000000000000000000, 0.0002224803680995706247, 0.0004449607361991412494, 0.0006674411042987119826, 0.0008899214723982824989, 0.001112401840497853015, 0.001334882208597423965, 0.001779842944796567817 ),
 .UNSPECIFIED. ) ;
#17833 = ORIENTED_EDGE ( 'NONE', *, *, #7694, .F. ) ;
#17834 = PLANE ( 'NONE',  #10825 ) ;
#17835 = CARTESIAN_POINT ( 'NONE',  ( -6.757590673342858345, 40.38754831509554322, 78.93286798364411538 ) ) ;
#17836 = CARTESIAN_POINT ( 'NONE',  ( -1.590937568396970203, 39.63064243629642647, 94.82933879953097289 ) ) ;
#17837 = EDGE_CURVE ( 'NONE', #6003, #8200, #4976, .T. ) ;
#17838 = ORIENTED_EDGE ( 'NONE', *, *, #5161, .T. ) ;
#17839 = CARTESIAN_POINT ( 'NONE',  ( -4.802822372555619168, 51.17292061857877172, 76.30694920102484957 ) ) ;
#17840 = DIRECTION ( 'NONE',  ( -0.000000000000000000, -0.000000000000000000, 1.000000000000000000 ) ) ;
#17841 = DIRECTION ( 'NONE',  ( 0.5670994908670431434, -0.8236492988270800453, -6.036271672687318437E-17 ) ) ;
#17842 = CARTESIAN_POINT ( 'NONE',  ( 4.394343283833276992, 39.11584570990505938, 95.10183880123797451 ) ) ;
#17843 = EDGE_CURVE ( 'NONE', #7860, #492, #12874, .T. ) ;
#17844 = UNCERTAINTY_MEASURE_WITH_UNIT (LENGTH_MEASURE( 1.000000000000000082E-05 ), #1678, 'distance_accuracy_value', 'NONE');
#17845 = CARTESIAN_POINT ( 'NONE',  ( -5.831867965436852153, 50.43760231366965030, 76.45423404125398292 ) ) ;
#17846 = CARTESIAN_POINT ( 'NONE',  ( -4.536948752023380216, 37.70884965637360153, 76.29326043209479735 ) ) ;
#17847 = FACE_OUTER_BOUND ( 'NONE', #12184, .T. ) ;
#17848 = DIRECTION ( 'NONE',  ( 1.540237394707284220E-16, 1.793354297423764243E-16, -1.000000000000000000 ) ) ;
#17849 = CARTESIAN_POINT ( 'NONE',  ( 8.535530527220215546, 40.37525097622586401, 79.30521328845429707 ) ) ;
#17850 = VERTEX_POINT ( 'NONE', #19356 ) ;
#17851 = DIRECTION ( 'NONE',  ( 3.893792155548169402E-16, 7.183611964723547524E-17, -1.000000000000000000 ) ) ;
#17852 = CYLINDRICAL_SURFACE ( 'NONE', #10623, 0.9921021478795020165 ) ;
#17853 = DIRECTION ( 'NONE',  ( 0.9585804129707224952, 0.2848220354341971516, 1.987228219138359058E-16 ) ) ;
#17854 = CARTESIAN_POINT ( 'NONE',  ( 6.275326403410204534, 49.93894407694084236, 77.80505143490314879 ) ) ;
#17855 = ORIENTED_EDGE ( 'NONE', *, *, #3242, .F. ) ;
#17856 = EDGE_CURVE ( 'NONE', #6568, #19622, #6154, .T. ) ;
#17857 = CARTESIAN_POINT ( 'NONE',  ( 7.843838371297746193, 40.46900263578136503, 75.68048307330049340 ) ) ;
#17858 = SURFACE_STYLE_USAGE ( .BOTH. , #9691 ) ;
#17859 = CARTESIAN_POINT ( 'NONE',  ( 31.22215374030650281, 45.56218137147968861, 72.80433879953100984 ) ) ;
#17860 = CARTESIAN_POINT ( 'NONE',  ( 4.270697848799480667, 51.45532176823032700, 79.05703599080955257 ) ) ;
#17861 = PLANE ( 'NONE',  #18136 ) ;
#17862 = PRODUCT_DEFINITION_SHAPE ( 'NONE', 'NONE',  #21043 ) ;
#17863 = CARTESIAN_POINT ( 'NONE',  ( 6.198496396448986090, 45.68315280215533392, 94.08621380123807398 ) ) ;
#17864 = CARTESIAN_POINT ( 'NONE',  ( 9.261243355884198891, 42.55025836209524215, 77.91040118276930571 ) ) ;
#17865 = CARTESIAN_POINT ( 'NONE',  ( 8.616653853821931719, 45.47331367307960193, 79.47125056423675460 ) ) ;
#17866 = CARTESIAN_POINT ( 'NONE',  ( 6.513673912301411129, 49.75206843158775172, 76.39262467917644983 ) ) ;
#17867 = CARTESIAN_POINT ( 'NONE',  ( -4.524181921268124462, 40.28999182795290324, 93.53933880123797451 ) ) ;
#17868 = VERTEX_POINT ( 'NONE', #11298 ) ;
#17869 = CARTESIAN_POINT ( 'NONE',  ( -4.638935325527024034, 37.97006185416216795, 79.53654225555244750 ) ) ;
#17870 = ORIENTED_EDGE ( 'NONE', *, *, #5279, .T. ) ;
#17871 = CARTESIAN_POINT ( 'NONE',  ( 8.898741081898894123, 41.46381605024582484, 78.92561463894257656 ) ) ;
#17872 = CARTESIAN_POINT ( 'NONE',  ( 5.308722110161348873, 50.82017868225404555, 78.91297906391670836 ) ) ;
#17873 = DIRECTION ( 'NONE',  ( -1.540237394707284467E-16, -1.793354297423764243E-16, 1.000000000000000000 ) ) ;
#17874 = CARTESIAN_POINT ( 'NONE',  ( 8.740212021938845055, 40.98869440064952130, 75.38759329643264095 ) ) ;
#17875 = ORIENTED_EDGE ( 'NONE', *, *, #8694, .T. ) ;
#17876 = ORIENTED_EDGE ( 'NONE', *, *, #7667, .T. ) ;
#17877 = CARTESIAN_POINT ( 'NONE',  ( -0.3307199010476375989, 52.21467244487229209, 75.52908203832478762 ) ) ;
#17878 = CARTESIAN_POINT ( 'NONE',  ( -4.009385194876762704, 46.27527268018315709, 94.20433879611698558 ) ) ;
#17879 = CARTESIAN_POINT ( 'NONE',  ( -4.592862224480081856, 51.32295045326188898, 75.97198585835440099 ) ) ;
#17880 = CARTESIAN_POINT ( 'NONE',  ( 4.765539811858917396, 51.17942285908035416, 75.44429008213492693 ) ) ;
#17881 = CARTESIAN_POINT ( 'NONE',  ( 2.522153740306511960, 47.62628298661745418, 45.55433879953100273 ) ) ;
#17882 = ORIENTED_EDGE ( 'NONE', *, *, #12341, .F. ) ;
#17883 = CARTESIAN_POINT ( 'NONE',  ( 4.577225057937401864, 52.10727814237509392, 78.46169174070733732 ) ) ;
#17884 = AXIS2_PLACEMENT_3D ( 'NONE', #13803, #15625, #10952 ) ;
#17885 = ORIENTED_EDGE ( 'NONE', *, *, #9893, .T. ) ;
#17886 = CARTESIAN_POINT ( 'NONE',  ( 1.352400422481993658, 50.46853102219002096, 93.07058880123798872 ) ) ;
#17887 = ADVANCED_FACE ( 'NONE', ( #9801 ), #10115, .F. ) ;
#17888 = CARTESIAN_POINT ( 'NONE',  ( 0.3279640439667347862, 52.35988168082469940, 76.44919174070734869 ) ) ;
#17889 = B_SPLINE_CURVE_WITH_KNOTS ( 'NONE', 3,
 ( #4541, #15940, #17426, #2638, #9139, #14122, #2851, #9354, #15839, #1251, #6241 ),
 .UNSPECIFIED., .F., .F.,
 ( 4, 1, 1, 1, 1, 1, 1, 1, 4 ),
 ( 0.000000000000000000, 0.1975140844462248968, 0.3638949407180063211, 0.4989527813026914393, 0.6061909113956662765, 0.6984313814761610173, 0.7906255499708312318, 0.8898677993983585832, 1.000000000000000000 ),
 .UNSPECIFIED. ) ;
#17890 = CARTESIAN_POINT ( 'NONE',  ( -3.533185125431083762, 36.21728222759317362, 78.38559710128819802 ) ) ;
#17891 = CARTESIAN_POINT ( 'NONE',  ( 8.334265403641039072, 41.66992841543623172, 75.99902581847530314 ) ) ;
#17892 = LINE ( 'NONE', #10140, #10604 ) ;
#17893 = EDGE_LOOP ( 'NONE', ( #18659, #9102, #5272, #709, #20856 ) ) ;
#17894 = CARTESIAN_POINT ( 'NONE',  ( 23.03948732994508575, 36.35905713404685002, 78.30433879953099563 ) ) ;
#17895 = ADVANCED_FACE ( 'NONE', ( #204 ), #9701, .T. ) ;
#17896 = ORIENTED_EDGE ( 'NONE', *, *, #6724, .T. ) ;
#17897 = AXIS2_PLACEMENT_3D ( 'NONE', #6809, #5105, #17780 ) ;
#17898 = FACE_BOUND ( 'NONE', #18263, .T. ) ;
#17899 = CARTESIAN_POINT ( 'NONE',  ( 2.263363662449358493, 49.77488197367694767, 94.44231768333818877 ) ) ;
#17900 = CARTESIAN_POINT ( 'NONE',  ( 4.394343283833276992, 39.11584570990505938, 93.85183880123797451 ) ) ;
#17901 = VERTEX_POINT ( 'NONE', #17771 ) ;
#17902 = CARTESIAN_POINT ( 'NONE',  ( 1.640639625673125712, 52.28578529826535259, 76.88709351585207230 ) ) ;
#17903 = CARTESIAN_POINT ( 'NONE',  ( 0.3821786226492924210, 35.36301154328572949, 78.57639762306027365 ) ) ;
#17904 = CARTESIAN_POINT ( 'NONE',  ( 5.889143815203415677, 51.13821660369377753, 76.04053158567903381 ) ) ;
#17905 = CARTESIAN_POINT ( 'NONE',  ( -2.914604833731050171, 51.60239615748798059, 78.10580938776615767 ) ) ;
#17906 = DIRECTION ( 'NONE',  ( 3.211742425186504723E-16, -5.922860397471811774E-17, 1.000000000000000000 ) ) ;
#17907 = VERTEX_POINT ( 'NONE', #13090 ) ;
#17908 = CARTESIAN_POINT ( 'NONE',  ( -1.997856540139665737, 38.86318974171943808, 92.55433879953103826 ) ) ;
#17909 = CARTESIAN_POINT ( 'NONE',  ( 2.522153740306511072, 49.16218137147969003, 50.55433879953100273 ) ) ;
#17910 = VERTEX_POINT ( 'NONE', #9912 ) ;
#17911 = CARTESIAN_POINT ( 'NONE',  ( 4.314250362499145730, 51.38751195140030603, 77.86982703766624070 ) ) ;
#17912 = CARTESIAN_POINT ( 'NONE',  ( -6.906571818728131085, 40.93480306606039676, 77.18350490445806145 ) ) ;
#17913 = CARTESIAN_POINT ( 'NONE',  ( -4.489196722361281644, 50.47725044336133493, 75.37785507730471579 ) ) ;
#17914 = CARTESIAN_POINT ( 'NONE',  ( -1.590937568396968871, 39.63064243629642647, 92.01683879611699979 ) ) ;
#17915 = VECTOR ( 'NONE', #12664, 1000.000000000000114 ) ;
#17916 = CARTESIAN_POINT ( 'NONE',  ( -3.628867371436362621, 48.69222599884265179, 91.07933879782399345 ) ) ;
#17917 = LINE ( 'NONE', #6418, #18327 ) ;
#17918 = CARTESIAN_POINT ( 'NONE',  ( 3.788215052820487205, 39.19523464621513398, 90.08681233796825438 ) ) ;
#17919 = CARTESIAN_POINT ( 'NONE',  ( 5.787239255393352266, 51.21348939705941206, 75.97375991483075097 ) ) ;
#17920 = ORIENTED_EDGE ( 'NONE', *, *, #12493, .T. ) ;
#17921 = CARTESIAN_POINT ( 'NONE',  ( 0.7060283986096523856, 52.21262887048612811, 79.54746358246200089 ) ) ;
#17922 = AXIS2_PLACEMENT_3D ( 'NONE', #9253, #3442, #5026 ) ;
#17923 = ORIENTED_EDGE ( 'NONE', *, *, #18961, .T. ) ;
#17924 = CARTESIAN_POINT ( 'NONE',  ( 11.22215374030650281, 42.76218137147968434, 66.20574467885104752 ) ) ;
#17925 = EDGE_CURVE ( 'NONE', #1396, #6827, #15130, .T. ) ;
#17926 = CARTESIAN_POINT ( 'NONE',  ( 35.92215374030650565, 47.36218137147962892, 93.55433879953098142 ) ) ;
#17927 = CARTESIAN_POINT ( 'NONE',  ( 9.353525637756030520, 42.82683421514393274, 78.50890480505780999 ) ) ;
#17928 = ORIENTED_EDGE ( 'NONE', *, *, #8796, .F. ) ;
#17929 = CARTESIAN_POINT ( 'NONE',  ( 2.043125170982144745, 38.48583871533720213, 93.92996380123798872 ) ) ;
#17930 = CARTESIAN_POINT ( 'NONE',  ( -5.679243918435854965, 37.80248940946448499, 75.65168154244369703 ) ) ;
#17932 = EDGE_CURVE ( 'NONE', #19237, #2125, #13196, .T. ) ;
#17931 = ORIENTED_EDGE ( 'NONE', *, *, #11068, .F. ) ;
#17933 = CIRCLE ( 'NONE', #1624, 4.200000000000001954 ) ;
#17934 = FACE_OUTER_BOUND ( 'NONE', #17133, .T. ) ;
#17935 = LINE ( 'NONE', #9866, #6097 ) ;
#17936 = CARTESIAN_POINT ( 'NONE',  ( -5.058133621542618030, 44.89684013992257405, 92.67996379953099506 ) ) ;
#17937 = ORIENTED_EDGE ( 'NONE', *, *, #426, .F. ) ;
#17938 = PLANE ( 'NONE',  #18948 ) ;
#17939 = CARTESIAN_POINT ( 'NONE',  ( 31.07218010054375412, 42.96218137147968008, 69.40574467885102194 ) ) ;
#17940 = CARTESIAN_POINT ( 'NONE',  ( 2.463659247115867590, 38.82793883177424732, 91.62621379782397923 ) ) ;
#17941 = EDGE_LOOP ( 'NONE', ( #3246, #15363, #12834, #20691 ) ) ;
#17942 = CARTESIAN_POINT ( 'NONE',  ( -3.777846259693483866, 51.36218137147968577, 54.55433879953099563 ) ) ;
#17943 = DIRECTION ( 'NONE',  ( -1.540237394707284467E-16, -1.793354297423764243E-16, 1.000000000000000000 ) ) ;
#17944 = CARTESIAN_POINT ( 'NONE',  ( 1.048114967784774310, 52.94689884418070136, 75.38689734427310896 ) ) ;
#17945 = CARTESIAN_POINT ( 'NONE',  ( 2.043125170982144745, 38.48583871533720213, 93.77371380123798872 ) ) ;
#17946 = EDGE_CURVE ( 'NONE', #15829, #10630, #5096, .T. ) ;
#17947 = ADVANCED_FACE ( 'NONE', ( #1912 ), #12131, .T. ) ;
#17948 = VECTOR ( 'NONE', #4273, 1000.000000000000000 ) ;
#17949 = DIRECTION ( 'NONE',  ( -5.782719800589917211E-18, -3.634796904962526723E-16, 1.000000000000000000 ) ) ;
#17950 = EDGE_CURVE ( 'NONE', #18376, #13576, #15111, .T. ) ;
#17951 = LINE ( 'NONE', #16362, #3378 ) ;
#17952 = DIRECTION ( 'NONE',  ( 0.3165065846431827645, 0.9485903129789529098, 0.000000000000000000 ) ) ;
#17953 = EDGE_CURVE ( 'NONE', #4353, #11695, #2547, .T. ) ;
#17954 = CARTESIAN_POINT ( 'NONE',  ( 4.162128861264472235, 36.86717768966805409, 75.77524573853747825 ) ) ;
#17955 = EDGE_CURVE ( 'NONE', #8338, #10035, #16703, .T. ) ;
#17956 = ORIENTED_EDGE ( 'NONE', *, *, #8138, .T. ) ;
#17957 = CARTESIAN_POINT ( 'NONE',  ( 9.539487329945082195, 27.61837231449496244, 75.00433879953101268 ) ) ;
#17958 = CARTESIAN_POINT ( 'NONE',  ( 9.346906861638174746, 42.80699732323137852, 76.23134092453109645 ) ) ;
#17959 = DIRECTION ( 'NONE',  ( -1.402518428993831676E-16, 1.000000000000000000, 0.000000000000000000 ) ) ;
#17960 = CARTESIAN_POINT ( 'NONE',  ( 6.484157998033387216, 49.78468859024245319, 78.34373887323252461 ) ) ;
#17961 = VECTOR ( 'NONE', #872, 1000.000000000000227 ) ;
#17962 = ORIENTED_EDGE ( 'NONE', *, *, #8570, .F. ) ;
#17963 = CARTESIAN_POINT ( 'NONE',  ( 5.466176856163651010, 50.69752978158682311, 78.92065061514911406 ) ) ;
#17964 = ORIENTED_EDGE ( 'NONE', *, *, #15219, .T. ) ;
#17965 = CARTESIAN_POINT ( 'NONE',  ( 5.722153740306477054, 44.16218185475116798, 93.64411094854725093 ) ) ;
#17966 = CARTESIAN_POINT ( 'NONE',  ( 10.77494014480653561, 42.76218137147968434, 69.40574467885102194 ) ) ;
#17967 = CARTESIAN_POINT ( 'NONE',  ( 4.686687817024941083, 51.22644301457940941, 79.43421539708423040 ) ) ;
#17968 = CARTESIAN_POINT ( 'NONE',  ( -3.154801521863568325, 47.83913663364971569, 94.11286078555450274 ) ) ;
#17969 = CARTESIAN_POINT ( 'NONE',  ( 4.393996117251955269, 36.11308595931626542, 76.73963291717792856 ) ) ;
#17970 = CARTESIAN_POINT ( 'NONE',  ( 8.631800694748326563, 43.02819682608614471, 77.50995918449682165 ) ) ;
#17971 = CARTESIAN_POINT ( 'NONE',  ( 4.143578761807024335, 51.51916996771892343, 78.37598241635205909 ) ) ;
#17972 = CARTESIAN_POINT ( 'NONE',  ( -4.883901707777988932, 37.21500215679002821, 76.12782976279942204 ) ) ;
#17973 = VECTOR ( 'NONE', #20972, 1000.000000000000000 ) ;
#17974 = VERTEX_POINT ( 'NONE', #13406 ) ;
#17975 = EDGE_CURVE ( 'NONE', #13018, #13741, #20192, .T. ) ;
#17976 = DIRECTION ( 'NONE',  ( -1.110223024625156540E-16, -1.000000000000000000, -5.922860397471808077E-17 ) ) ;
#17977 = CARTESIAN_POINT ( 'NONE',  ( -5.838300394258943093, 50.43300593553962585, 78.21416447440572028 ) ) ;
#17978 = CARTESIAN_POINT ( 'NONE',  ( -4.344504932464893443, 37.57120742909659583, 78.93669174070734584 ) ) ;
#17979 = CARTESIAN_POINT ( 'NONE',  ( 8.921473627994183531, 41.53194693301924190, 77.48121952543638713 ) ) ;
#17980 = CARTESIAN_POINT ( 'NONE',  ( 8.387827792284632267, 39.93257650953714943, 76.58175473889373563 ) ) ;
#17981 = ORIENTED_EDGE ( 'NONE', *, *, #16236, .F. ) ;
#17982 = VERTEX_POINT ( 'NONE', #15000 ) ;
#17983 = CIRCLE ( 'NONE', #10198, 3.999999999999996447 ) ;
#17984 = CARTESIAN_POINT ( 'NONE',  ( 6.402690229413289025, 38.46820081115981083, 76.05683950549904182 ) ) ;
#17985 = CARTESIAN_POINT ( 'NONE',  ( 0.2833753639608733721, 52.20780802782073238, 79.53425070713537082 ) ) ;
#17986 = CARTESIAN_POINT ( 'NONE',  ( 7.823713835575672348, 40.42945125626696523, 79.18036419938457016 ) ) ;
#17987 = CARTESIAN_POINT ( 'NONE',  ( -3.557579061748611160, 36.23530104570325250, 76.03954924220039402 ) ) ;
#17988 = LINE ( 'NONE', #15, #20110 ) ;
#17989 = ORIENTED_EDGE ( 'NONE', *, *, #9076, .T. ) ;
#17990 =( BOUNDED_CURVE ( )  B_SPLINE_CURVE ( 3, ( #6540, #13046, #1870, #18240 ),
 .UNSPECIFIED., .F., .F. ) 
 B_SPLINE_CURVE_WITH_KNOTS ( ( 4, 4 ),
 ( 1.230959417340771189, 1.276280841686757483 ),
 .UNSPECIFIED. ) 
 CURVE ( )  GEOMETRIC_REPRESENTATION_ITEM ( )  RATIONAL_B_SPLINE_CURVE ( ( 1.000000000000000000, 0.9998288380325437430, 0.9998288380325437430, 1.000000000000000000 ) ) 
 REPRESENTATION_ITEM ( '' )  );
#17991 = DIRECTION ( 'NONE',  ( 0.007885122365275663500, 0.9999689119394085113, 1.805443505845543142E-16 ) ) ;
#17992 = CIRCLE ( 'NONE', #20350, 8.199999999999995737 ) ;
#17993 = CIRCLE ( 'NONE', #4057, 8.199999999999995737 ) ;
#17994 = EDGE_LOOP ( 'NONE', ( #15029, #1342, #6741, #1265, #73, #4139 ) ) ;
#17995 = CARTESIAN_POINT ( 'NONE',  ( -4.567115856812060670, 47.10047254335474065, 92.05496380123798872 ) ) ;
#17996 = VECTOR ( 'NONE', #2187, 1000.000000000000000 ) ;
#17997 = CARTESIAN_POINT ( 'NONE',  ( 0.5221537403065010796, 44.16218137147969003, 45.55433879953098852 ) ) ;
#17998 = DIRECTION ( 'NONE',  ( 1.000000000000000000, -1.110223024625156540E-16, 1.779391786395883043E-16 ) ) ;
#17999 = AXIS2_PLACEMENT_3D ( 'NONE', #14511, #3834, #8530 ) ;
#18000 = VECTOR ( 'NONE', #19304, 1000.000000000000000 ) ;
#18001 = CARTESIAN_POINT ( 'NONE',  ( 7.691771551572208487, 40.18266124458227750, 72.45433879953087342 ) ) ;
#18002 = VERTEX_POINT ( 'NONE', #18608 ) ;
#18003 = DIRECTION ( 'NONE',  ( -0.9429220365244147528, 0.3330135628418914862, -8.551124769255465366E-17 ) ) ;
#18004 = ORIENTED_EDGE ( 'NONE', *, *, #14148, .T. ) ;
#18005 = AXIS2_PLACEMENT_3D ( 'NONE', #20975, #20577, #17702 ) ;
#18006 = LINE ( 'NONE', #15030, #12918 ) ;
#18007 = CARTESIAN_POINT ( 'NONE',  ( 28.52215374030649642, 44.16218137147969003, 87.05433879953100984 ) ) ;
#18008 = DIRECTION ( 'NONE',  ( -0.5941461771851691553, -0.8043570849667760481, -2.357623395011396791E-16 ) ) ;
#18009 = ORIENTED_EDGE ( 'NONE', *, *, #9383, .F. ) ;
#18010 = CARTESIAN_POINT ( 'NONE',  ( -5.616859571223690395, 50.59123944021462904, 79.13778479689705136 ) ) ;
#18011 = CARTESIAN_POINT ( 'NONE',  ( -10.17784625969349754, 51.36218137147968577, 80.55433879953099563 ) ) ;
#18012 = CARTESIAN_POINT ( 'NONE',  ( 5.939788499136119171, 51.10080741576499719, 76.32243632687685420 ) ) ;
#18013 = CARTESIAN_POINT ( 'NONE',  ( -4.383473025373059606, 51.47257230871590394, 78.45066232894264147 ) ) ;
#18014 = LINE ( 'NONE', #11122, #20800 ) ;
#18015 = ORIENTED_EDGE ( 'NONE', *, *, #8600, .T. ) ;
#18016 = LINE ( 'NONE', #16435, #15301 ) ;
#18017 = VECTOR ( 'NONE', #6273, 1000.000000000000000 ) ;
#18018 = CARTESIAN_POINT ( 'NONE',  ( 0.7261808065621055963, 52.35991697419684243, 76.81167236361466166 ) ) ;
#18019 = ORIENTED_EDGE ( 'NONE', *, *, #19537, .F. ) ;
#18020 = CARTESIAN_POINT ( 'NONE',  ( 4.685757199431944464, 52.02710982139440432, 77.94290914044947272 ) ) ;
#18021 = DIRECTION ( 'NONE',  ( -1.621236893436268647E-16, -2.273814620809075225E-32, 1.000000000000000000 ) ) ;
#18022 = CARTESIAN_POINT ( 'NONE',  ( -4.204074076407136040, 37.46120757759153719, 77.13799123457000917 ) ) ;
#18023 = CARTESIAN_POINT ( 'NONE',  ( 0.7582201636353285146, 49.56899138526064519, 92.71996379611701400 ) ) ;
#18024 = VECTOR ( 'NONE', #6802, 1000.000000000000000 ) ;
#18025 = CARTESIAN_POINT ( 'NONE',  ( 8.951667845840693971, 41.62244091939069790, 77.14698585835439815 ) ) ;
#18026 = CARTESIAN_POINT ( 'NONE',  ( 5.482029497793807771, 37.63747020982715696, 76.09175310361966638 ) ) ;
#18027 = CARTESIAN_POINT ( 'NONE',  ( -1.477846259693494702, 50.16218137147969713, 85.15433879953098995 ) ) ;
#18028 = CARTESIAN_POINT ( 'NONE',  ( 5.579217223280415361, 50.61251095053976456, 76.36217657474753651 ) ) ;
#18029 = ORIENTED_EDGE ( 'NONE', *, *, #11688, .T. ) ;
#18030 = FACE_OUTER_BOUND ( 'NONE', #20359, .T. ) ;
#18031 = DIRECTION ( 'NONE',  ( 3.893792155548169402E-16, 7.183611964723547524E-17, -1.000000000000000000 ) ) ;
#18032 = VERTEX_POINT ( 'NONE', #18506 ) ;
#18033 = CARTESIAN_POINT ( 'NONE',  ( -1.854173455793825864, 49.13976469971944994, 93.55877693069184886 ) ) ;
#18034 = EDGE_CURVE ( 'NONE', #3547, #8376, #16706, .T. ) ;
#18035 = DIRECTION ( 'NONE',  ( -3.211742425186504723E-16, 5.922860397471811774E-17, -1.000000000000000000 ) ) ;
#18036 = CARTESIAN_POINT ( 'NONE',  ( 9.335797811945472091, 42.77370279655738017, 78.83313045764568017 ) ) ;
#18037 = PRODUCT_DEFINITION_SHAPE ( 'NONE', 'NONE',  #8194 ) ;
#18038 = ORIENTED_EDGE ( 'NONE', *, *, #13153, .T. ) ;
#18039 = CARTESIAN_POINT ( 'NONE',  ( 31.07218010054375412, 45.56218137147968861, 70.80574467885102763 ) ) ;
#18040 = CARTESIAN_POINT ( 'NONE',  ( -4.891113921371359474, 38.15633602453890916, 75.45005776384208218 ) ) ;
#18041 = VERTEX_POINT ( 'NONE', #7328 ) ;
#18042 = CARTESIAN_POINT ( 'NONE',  ( 1.514255888186008425, 52.36218137147968577, 52.53721119516358584 ) ) ;
#18043 = CARTESIAN_POINT ( 'NONE',  ( -1.579458713458412822, 38.67424504376464967, 92.55433879953098142 ) ) ;
#18044 = CARTESIAN_POINT ( 'NONE',  ( -2.904223097202481174, 48.62752260303690122, 93.77371379953099506 ) ) ;
#18045 = VERTEX_POINT ( 'NONE', #10548 ) ;
#18046 = DIRECTION ( 'NONE',  ( 0.8136266022444373913, 0.5813877811927010697, 2.295812393977109593E-16 ) ) ;
#18047 = CARTESIAN_POINT ( 'NONE',  ( -4.537329489133296256, 36.95900321965768143, 78.11020518223413944 ) ) ;
#18048 = CARTESIAN_POINT ( 'NONE',  ( -1.590937568396969759, 39.63064243629642647, 93.57933879953097289 ) ) ;
#18049 = ORIENTED_EDGE ( 'NONE', *, *, #5066, .T. ) ;
#18050 = CARTESIAN_POINT ( 'NONE',  ( -7.854101642381717596, 41.46402583572638889, 78.93502120504803088 ) ) ;
#18051 = CARTESIAN_POINT ( 'NONE',  ( 0.5221537403065112937, 44.16218137147969713, 46.35433879953098568 ) ) ;
#18052 = CARTESIAN_POINT ( 'NONE',  ( 4.100190290135135029, 51.54036911970691648, 72.45433879953087342 ) ) ;
#18053 = VECTOR ( 'NONE', #6945, 1000.000000000000000 ) ;
#18054 = DIRECTION ( 'NONE',  ( 1.000000000000000000, 0.000000000000000000, 0.000000000000000000 ) ) ;
#18055 = EDGE_CURVE ( 'NONE', #6977, #10346, #18718, .T. ) ;
#18056 = CARTESIAN_POINT ( 'NONE',  ( 0.3278485956581845273, 52.34524085292903095, 77.10139762306027933 ) ) ;
#18057 = ORIENTED_EDGE ( 'NONE', *, *, #14966, .T. ) ;
#18058 = CARTESIAN_POINT ( 'NONE',  ( 4.318075228076872385, 36.97861125383128922, 75.61597629374708163 ) ) ;
#18059 = ADVANCED_FACE ( 'NONE', ( #16907 ), #2333, .T. ) ;
#18060 = DIRECTION ( 'NONE',  ( -1.110223024625156540E-16, -1.000000000000000000, -5.922860397471808077E-17 ) ) ;
#18061 = ORIENTED_EDGE ( 'NONE', *, *, #16366, .T. ) ;
#18062 = VECTOR ( 'NONE', #4552, 1000.000000000000114 ) ;
#18063 = DIRECTION ( 'NONE',  ( -0.3165065846431827645, -0.9485903129789529098, 0.000000000000000000 ) ) ;
#18064 = DIRECTION ( 'NONE',  ( 1.000000000000000000, 0.000000000000000000, 0.000000000000000000 ) ) ;
#18065 = CARTESIAN_POINT ( 'NONE',  ( 0.5221537403064985261, 44.16218137147969003, 96.05433879953096721 ) ) ;
#18066 = CARTESIAN_POINT ( 'NONE',  ( 6.486188022505683826, 49.78318909293913919, 78.43783143115764744 ) ) ;
#18067 = AXIS2_PLACEMENT_3D ( 'NONE', #13172, #19332, #11589 ) ;
#18068 = EDGE_CURVE ( 'NONE', #10195, #3440, #1403, .T. ) ;
#18069 = ORIENTED_EDGE ( 'NONE', *, *, #10762, .T. ) ;
#18070 = EDGE_CURVE ( 'NONE', #19191, #17483, #8828, .T. ) ;
#18071 = CARTESIAN_POINT ( 'NONE',  ( 28.43948732994508788, 45.16218137147969003, 74.70433879953100131 ) ) ;
#18072 = VERTEX_POINT ( 'NONE', #2445 ) ;
#18073 = CARTESIAN_POINT ( 'NONE',  ( -2.167873396875370950, 37.04784696823259793, 72.45432679953087529 ) ) ;
#18074 = CARTESIAN_POINT ( 'NONE',  ( 4.728442938187240152, 51.99557958566231264, 77.51131257087278925 ) ) ;
#18075 = EDGE_CURVE ( 'NONE', #6065, #14337, #69, .T. ) ;
#18076 = CARTESIAN_POINT ( 'NONE',  ( -0.9259701616170338268, 52.84221263810348290, 76.43547538781149342 ) ) ;
#18077 = DIRECTION ( 'NONE',  ( 1.540237394707284220E-16, 1.793354297423764243E-16, -1.000000000000000000 ) ) ;
#18078 = CARTESIAN_POINT ( 'NONE',  ( 6.660594192354430731, 43.89417127335556046, 93.11058879782397923 ) ) ;
#18079 = CARTESIAN_POINT ( 'NONE',  ( 5.568489401881125289, 48.03437091500647682, 94.16433880123805977 ) ) ;
#18080 = VECTOR ( 'NONE', #2592, 1000.000000000000114 ) ;
#18081 = CARTESIAN_POINT ( 'NONE',  ( 4.133675539746122674, 51.51007735721194791, 76.08931382966170531 ) ) ;
#18082 = CARTESIAN_POINT ( 'NONE',  ( -3.068202438178982749, 36.79865119415181596, 76.30596599901106458 ) ) ;
#18083 = VECTOR ( 'NONE', #5727, 1000.000000000000114 ) ;
#18084 = CARTESIAN_POINT ( 'NONE',  ( 2.043125170982144745, 38.48583871533720213, 91.27371380123798872 ) ) ;
#18085 = ORIENTED_EDGE ( 'NONE', *, *, #4880, .T. ) ;
#18086 = DIRECTION ( 'NONE',  ( 1.540237394707284220E-16, 1.793354297423764243E-16, -1.000000000000000000 ) ) ;
#18087 = CARTESIAN_POINT ( 'NONE',  ( 8.950289981099260217, 41.61831137135051506, 78.71610475470291135 ) ) ;
#18088 = CARTESIAN_POINT ( 'NONE',  ( -4.796313072339920325, 37.15030396007738744, 78.92026643871187730 ) ) ;
#18089 = AXIS2_PLACEMENT_3D ( 'NONE', #513, #19969, #20290 ) ;
#18090 = DIRECTION ( 'NONE',  ( 1.110223024625156540E-16, 1.000000000000000000, 5.922860397471808077E-17 ) ) ;
#18091 = EDGE_CURVE ( 'NONE', #10540, #54, #13818, .T. ) ;
#18092 = AXIS2_PLACEMENT_3D ( 'NONE', #775, #13753, #7473 ) ;
#18093 = CARTESIAN_POINT ( 'NONE',  ( 8.550070540977731781, 40.41882831985841307, 75.56834740413086138 ) ) ;
#18094 = ORIENTED_EDGE ( 'NONE', *, *, #16384, .T. ) ;
#18095 = CARTESIAN_POINT ( 'NONE',  ( 0.6452642261158869630, 52.96739513210086159, 79.54845644658969661 ) ) ;
#18096 = CARTESIAN_POINT ( 'NONE',  ( 6.435710703716235770, 38.49179603313996978, 77.55645576794258034 ) ) ;
#18097 = CARTESIAN_POINT ( 'NONE',  ( 5.394152393224890041, 50.75790946820724514, 75.36022115247205022 ) ) ;
#18098 = EDGE_CURVE ( 'NONE', #17279, #5762, #4131, .T. ) ;
#18099 = CARTESIAN_POINT ( 'NONE',  ( 0.8505168181936991756, 52.95605297189983673, 76.43141495382415940 ) ) ;
#18100 = ORIENTED_EDGE ( 'NONE', *, *, #2, .T. ) ;
#18101 = DIRECTION ( 'NONE',  ( -1.540237394707284220E-16, -1.793354297423764243E-16, 1.000000000000000000 ) ) ;
#18102 = EDGE_CURVE ( 'NONE', #3603, #13955, #10661, .T. ) ;
#18103 = EDGE_CURVE ( 'NONE', #16344, #18958, #19878, .T. ) ;
#18104 = LINE ( 'NONE', #15017, #12916 ) ;
#18105 = EDGE_LOOP ( 'NONE', ( #19847, #16080, #370, #1110 ) ) ;
#18106 = CARTESIAN_POINT ( 'NONE',  ( 5.146041124512939824, 40.41782456190201600, 90.15009067557426192 ) ) ;
#18107 = CARTESIAN_POINT ( 'NONE',  ( 0.5221537403065100724, 44.16218137147969713, 53.55433879953100273 ) ) ;
#18108 = AXIS2_PLACEMENT_3D ( 'NONE', #17696, #14400, #36 ) ;
#18109 = CARTESIAN_POINT ( 'NONE',  ( -5.784195910403845176, 44.99242805365518194, 95.88308880123798872 ) ) ;
#18110 = CARTESIAN_POINT ( 'NONE',  ( 8.627730818565934712, 42.92075920536279199, 79.03125282521155270 ) ) ;
#18111 = ORIENTED_EDGE ( 'NONE', *, *, #20955, .T. ) ;
#18112 = CARTESIAN_POINT ( 'NONE',  ( 0.9498231628969826534, 40.36218137147969998, 46.15433879953098284 ) ) ;
#18113 = ORIENTED_EDGE ( 'NONE', *, *, #17191, .T. ) ;
#18114 = DIRECTION ( 'NONE',  ( -1.301042606982606060E-16, -1.000000000000000000, 0.000000000000000000 ) ) ;
#18115 = CARTESIAN_POINT ( 'NONE',  ( -5.677846259693490438, 44.16218137147969003, 80.55433879953099563 ) ) ;
#18116 = CARTESIAN_POINT ( 'NONE',  ( 0.3821786226492928651, 35.36301154328572949, 75.45433879953087342 ) ) ;
#18117 =( BOUNDED_SURFACE ( )  B_SPLINE_SURFACE ( 1, 2, ( 
 ( #6528, #9644, #7926, #17916, #6631, #1762, #19297, #8347, #10058, #11240, #11656, #19404, #14829, #3239, #13132, #8029, #9844, #4711, #3554, #19718, #11443, #14518, #13034, #16124, #17711, #16333, #19607, #14728, #20982, #246, #4823, #17814, #18133, #16224, #6735, #14624, #5030, #149, #11549, #3446, #9959, #5136, #10384, #10600, #564, #16751, #8449, #13546, #16645, #20021, #3861, #14931, #15047, #20234, #11757, #5345, #16954, #10490, #18335, #787, #8883, #18231, #5456 ),
 ( #3651, #7047, #355, #2172, #1958, #6842, #11969, #15152, #3752, #10275, #18446, #5666, #678, #16853, #11857, #7157, #18551, #2065, #5241, #8771, #5568, #2270, #2383, #8671, #13348, #19819, #6942, #15259, #10163, #19919, #12071, #15371, #13659, #8562, #7268, #12176, #461, #20133, #18654, #13447, #3964, #13762, #4073, #17068, #17375, #7373, #13864, #12590, #10802, #7596, #14079, #14171, #11009, #12288, #17481, #12389, #1107, #15472, #20560, #20344, #1311, #18867, #20459 ) ),
 .UNSPECIFIED., .F., .F., .F. ) 
 B_SPLINE_SURFACE_WITH_KNOTS ( ( 2, 2 ),
 ( 3, 2, 2, 2, 2, 2, 2, 2, 2, 2, 2, 2, 2, 2, 2, 2, 2, 2, 2, 2, 2, 2, 2, 2, 2, 2, 2, 2, 2, 2, 2, 3 ),
 ( 0.000000000000000000, 1.000000000000000000 ),
 ( 0.000000000000000000, 0.03125000000000000000, 0.06250000000000000000, 0.09375000000000000000, 0.1250000000000000000, 0.1562500000000000000, 0.1875000000000000000, 0.2187500000000000000, 0.2500000000000000000, 0.2812500000000000000, 0.3125000000000000000, 0.3437500000000000000, 0.3750000000000000000, 0.4062500000000000000, 0.4375000000000000000, 0.4687500000000000000, 0.5000000000000000000, 0.5312500000000000000, 0.5625000000000000000, 0.5937500000000000000, 0.6250000000000000000, 0.6562500000000000000, 0.6875000000000000000, 0.7187500000000000000, 0.7500000000000000000, 0.7812500000000000000, 0.8125000000000000000, 0.8437500000000000000, 0.8750000000000000000, 0.9062500000000000000, 0.9200238152893590593, 0.9292240534422526732 ),
 .UNSPECIFIED. ) 
 GEOMETRIC_REPRESENTATION_ITEM ( )  RATIONAL_B_SPLINE_SURFACE ( (
 ( 1.000000000000000000, 0.9238795325112867385, 1.000000000000000000, 0.9238795325112867385, 1.000000000000000000, 0.9238795325112867385, 1.000000000000000000, 0.9238795325112867385, 1.000000000000000000, 0.9238795325112867385, 1.000000000000000000, 0.9238795325112867385, 1.000000000000000000, 0.9238795325112867385, 1.000000000000000000, 0.9238795325112867385, 1.000000000000000000, 0.9238795325112867385, 1.000000000000000000, 0.9238795325112867385, 1.000000000000000000, 0.9238795325112867385, 1.000000000000000000, 0.9238795325112867385, 1.000000000000000000, 0.9238795325112867385, 1.000000000000000000, 0.9238795325112867385, 1.000000000000000000, 0.9238795325112867385, 1.000000000000000000, 0.9238795325112867385, 1.000000000000000000, 0.9238795325112867385, 1.000000000000000000, 0.9238795325112867385, 1.000000000000000000, 0.9238795325112867385, 1.000000000000000000, 0.9238795325112867385, 1.000000000000000000, 0.9238795325112867385, 1.000000000000000000, 0.9238795325112867385, 1.000000000000000000, 0.9238795325112867385, 1.000000000000000000, 0.9238795325112867385, 1.000000000000000000, 0.9238795325112867385, 1.000000000000000000, 0.9238795325112867385, 1.000000000000000000, 0.9238795325112867385, 1.000000000000000000, 0.9238795325112867385, 1.000000000000000000, 0.9238795325112867385, 1.000000000000000000, 0.9664489837142656858, 0.9624739994982902669, 0.9624739994982902669, 0.9624739994982902669),
 ( 1.000000000000000000, 0.9238795325112867385, 1.000000000000000000, 0.9238795325112867385, 1.000000000000000000, 0.9238795325112867385, 1.000000000000000000, 0.9238795325112867385, 1.000000000000000000, 0.9238795325112867385, 1.000000000000000000, 0.9238795325112867385, 1.000000000000000000, 0.9238795325112867385, 1.000000000000000000, 0.9238795325112867385, 1.000000000000000000, 0.9238795325112867385, 1.000000000000000000, 0.9238795325112867385, 1.000000000000000000, 0.9238795325112867385, 1.000000000000000000, 0.9238795325112867385, 1.000000000000000000, 0.9238795325112867385, 1.000000000000000000, 0.9238795325112867385, 1.000000000000000000, 0.9238795325112867385, 1.000000000000000000, 0.9238795325112867385, 1.000000000000000000, 0.9238795325112867385, 1.000000000000000000, 0.9238795325112867385, 1.000000000000000000, 0.9238795325112867385, 1.000000000000000000, 0.9238795325112867385, 1.000000000000000000, 0.9238795325112867385, 1.000000000000000000, 0.9238795325112867385, 1.000000000000000000, 0.9238795325112867385, 1.000000000000000000, 0.9238795325112867385, 1.000000000000000000, 0.9238795325112867385, 1.000000000000000000, 0.9238795325112867385, 1.000000000000000000, 0.9238795325112867385, 1.000000000000000000, 0.9238795325112867385, 1.000000000000000000, 0.9238795325112867385, 1.000000000000000000, 0.9664489837142656858, 0.9624739994982902669, 0.9624739994982902669, 0.9624739994982902669) ) ) 
 REPRESENTATION_ITEM ( '' )  SURFACE ( )  );
#18118 = ORIENTED_EDGE ( 'NONE', *, *, #1313, .F. ) ;
#18119 = DIRECTION ( 'NONE',  ( -0.5941461771851693774, -0.8043570849667760481, -2.357623395011396791E-16 ) ) ;
#18120 = CARTESIAN_POINT ( 'NONE',  ( -5.919594526472893747, 37.98002672170838423, 78.92638042842689572 ) ) ;
#18121 = VECTOR ( 'NONE', #16116, 1000.000000000000000 ) ;
#18122 = CARTESIAN_POINT ( 'NONE',  ( 3.694606274243302568, 39.25854522838572080, 92.55433879953095300 ) ) ;
#18123 = CARTESIAN_POINT ( 'NONE',  ( -4.393892947181490705, 51.46512661408927869, 78.70491066849456274 ) ) ;
#18124 = ADVANCED_FACE ( 'NONE', ( #8631 ), #11812, .F. ) ;
#18125 = CARTESIAN_POINT ( 'NONE',  ( 0.3279818009034626280, 52.35625691656657210, 78.52223653336807274 ) ) ;
#18126 = ORIENTED_EDGE ( 'NONE', *, *, #5047, .F. ) ;
#18127 = CARTESIAN_POINT ( 'NONE',  ( -4.219550833609926777, 50.84278967315511721, 75.97260225988416948 ) ) ;
#18128 = EDGE_LOOP ( 'NONE', ( #14782, #4258, #1979, #9659, #17526, #5356, #4840, #567, #14555, #16145, #13463 ) ) ;
#18129 = DIRECTION ( 'NONE',  ( 0.9999689119394086223, -0.007885122365275665235, 1.526048693634353392E-16 ) ) ;
#18130 = CARTESIAN_POINT ( 'NONE',  ( -7.704497869805115862, 40.97402890596596592, 76.84875211988632770 ) ) ;
#18131 = CARTESIAN_POINT ( 'NONE',  ( -4.385150316929264491, 37.59252787896735981, 77.30162809418146708 ) ) ;
#18132 = CARTESIAN_POINT ( 'NONE',  ( -3.190985070539315682, 47.80295308497395013, 95.05235256388647258 ) ) ;
#18133 = CARTESIAN_POINT ( 'NONE',  ( 2.921181103050038974, 49.30691215337508737, 93.34496379782397923 ) ) ;
#18134 = CARTESIAN_POINT ( 'NONE',  ( 5.433479250907716995, 37.60277798094034551, 76.01697444493925104 ) ) ;
#18135 = CARTESIAN_POINT ( 'NONE',  ( -7.079689812751086997, 47.05182882866842675, 78.14247693707426379 ) ) ;
#18136 = AXIS2_PLACEMENT_3D ( 'NONE', #11602, #6679, #3285 ) ;
#18137 = VERTEX_POINT ( 'NONE', #16811 ) ;
#18138 = LINE ( 'NONE', #14938, #1358 ) ;
#18139 = CARTESIAN_POINT ( 'NONE',  ( 5.410058914415630582, 36.83912723373610731, 78.11840496518735222 ) ) ;
#18140 = VERTEX_POINT ( 'NONE', #8723 ) ;
#18141 = FACE_OUTER_BOUND ( 'NONE', #19098, .T. ) ;
#18142 = ADVANCED_FACE ( 'NONE', ( #19036 ), #9043, .T. ) ;
#18143 = LINE ( 'NONE', #2075, #11633 ) ;
#18144 = CARTESIAN_POINT ( 'NONE',  ( 5.025485839985549319, 41.56218137147963887, 93.22683879953099506 ) ) ;
#18145 = ORIENTED_EDGE ( 'NONE', *, *, #6533, .T. ) ;
#18146 = CARTESIAN_POINT ( 'NONE',  ( 6.882736312352589536, 37.89144858414100270, 76.69330938776616335 ) ) ;
#18147 = CARTESIAN_POINT ( 'NONE',  ( -5.420941400696308143, 38.54769824076353046, 75.91870325888974946 ) ) ;
#18148 = VERTEX_POINT ( 'NONE', #4339 ) ;
#18149 = CARTESIAN_POINT ( 'NONE',  ( -0.9436870690626151248, 52.23009998296728895, 77.21536821129558348 ) ) ;
#18150 = CARTESIAN_POINT ( 'NONE',  ( 0.3329543312200850536, 52.96014725284622671, 76.39696649187393973 ) ) ;
#18151 = CARTESIAN_POINT ( 'NONE',  ( -3.981178359372548492, 46.76218137147973408, 95.10183879953099506 ) ) ;
#18152 = ORIENTED_EDGE ( 'NONE', *, *, #4784, .F. ) ;
#18153 = FACE_OUTER_BOUND ( 'NONE', #12737, .T. ) ;
#18154 = ORIENTED_EDGE ( 'NONE', *, *, #14178, .F. ) ;
#18155 = DIRECTION ( 'NONE',  ( -0.000000000000000000, -0.000000000000000000, 1.000000000000000000 ) ) ;
#18156 = CARTESIAN_POINT ( 'NONE',  ( 0.9589043286300715785, 52.95179583173001703, 75.37608287192134071 ) ) ;
#18157 = CARTESIAN_POINT ( 'NONE',  ( 0.000000000000000000, 0.000000000000000000, 0.000000000000000000 ) ) ;
#18158 = CARTESIAN_POINT ( 'NONE',  ( 6.090066878584988075, 50.06496988346189880, 75.53514883118299394 ) ) ;
#18159 = CYLINDRICAL_SURFACE ( 'NONE', #6110, 4.000000000000000000 ) ;
#18160 = ADVANCED_FACE ( 'NONE', ( #5842 ), #15952, .T. ) ;
#18161 = PLANE ( 'NONE',  #1434 ) ;
#18162 = ORIENTED_EDGE ( 'NONE', *, *, #12739, .T. ) ;
#18163 = CARTESIAN_POINT ( 'NONE',  ( 4.853207525418807400, 37.36099720106794564, 75.39318197153889400 ) ) ;
#18164 = CARTESIAN_POINT ( 'NONE',  ( 2.522153740306507963, 50.16218137147969713, 69.55433879953100984 ) ) ;
#18165 = ORIENTED_EDGE ( 'NONE', *, *, #17335, .T. ) ;
#18166 = CARTESIAN_POINT ( 'NONE',  ( 6.882736312352589536, 37.89144858414100270, 77.26022115247205591 ) ) ;
#18167 = CARTESIAN_POINT ( 'NONE',  ( 8.452544761179964894, 42.49095542139739479, 75.50722976489458915 ) ) ;
#18168 = LINE ( 'NONE', #14977, #11620 ) ;
#18169 = CARTESIAN_POINT ( 'NONE',  ( -7.202951829524388394, 41.41213674333113914, 78.65672070501008761 ) ) ;
#18170 = ORIENTED_EDGE ( 'NONE', *, *, #11282, .T. ) ;
#18171 = ORIENTED_EDGE ( 'NONE', *, *, #14367, .F. ) ;
#18172 = ADVANCED_FACE ( 'NONE', ( #14234 ), #4448, .F. ) ;
#18173 = CARTESIAN_POINT ( 'NONE',  ( -4.895593109503407980, 37.22363812428621088, 78.18375056423674607 ) ) ;
#18174 = VERTEX_POINT ( 'NONE', #4233 ) ;
#18175 = CARTESIAN_POINT ( 'NONE',  ( -4.006646489220814011, 48.09791109810387155, 80.45433879953087342 ) ) ;
#18176 = CARTESIAN_POINT ( 'NONE',  ( -2.167873396875370950, 37.04784696823259793, 75.45433879953087342 ) ) ;
#18177 = CARTESIAN_POINT ( 'NONE',  ( 4.367780705229349358, 51.33715330180078951, 77.58315289018165117 ) ) ;
#18178 = CARTESIAN_POINT ( 'NONE',  ( 8.352692957205995583, 41.72820301203469739, 77.48007297599048115 ) ) ;
#18179 = LINE ( 'NONE', #6803, #9966 ) ;
#18180 = CARTESIAN_POINT ( 'NONE',  ( 6.660594192354428955, 43.89417127335556046, 94.36058879782399345 ) ) ;
#18181 = CARTESIAN_POINT ( 'NONE',  ( 8.211401091253357265, 41.32387017323333112, 76.34522901481825841 ) ) ;
#18182 = DIRECTION ( 'NONE',  ( 1.110223024625156540E-16, 1.000000000000000000, 5.922860397471808077E-17 ) ) ;
#18183 = DIRECTION ( 'NONE',  ( 1.402518428993831676E-16, -1.000000000000000000, 0.000000000000000000 ) ) ;
#18184 = CARTESIAN_POINT ( 'NONE',  ( 6.198496396448986090, 45.68315280215533392, 90.33621380123798872 ) ) ;
#18185 = CARTESIAN_POINT ( 'NONE',  ( -4.567115856812060670, 47.10047254335474065, 90.80496380123797451 ) ) ;
#18186 = VERTEX_POINT ( 'NONE', #15848 ) ;
#18187 = CARTESIAN_POINT ( 'NONE',  ( 3.961507247562192635, 36.71833509068318335, 76.73963291717792856 ) ) ;
#18188 = CARTESIAN_POINT ( 'NONE',  ( 0.8377421044266869510, 51.35991668224300355, 77.76169174070734869 ) ) ;
#18189 = CARTESIAN_POINT ( 'NONE',  ( 8.563160678057862185, 42.55264511967046559, 75.54928777999336376 ) ) ;
#18190 = CARTESIAN_POINT ( 'NONE',  ( 8.951218635964366399, 41.62109460889399770, 77.24172240072661566 ) ) ;
#18191 = CARTESIAN_POINT ( 'NONE',  ( -4.477846259693480491, 50.66141209518846011, 53.55433879953099563 ) ) ;
#18192 = EDGE_CURVE ( 'NONE', #1841, #5158, #12293, .T. ) ;
#18193 = CARTESIAN_POINT ( 'NONE',  ( 8.722153740306486824, 51.36218137147968577, 95.05433879953098142 ) ) ;
#18194 = EDGE_LOOP ( 'NONE', ( #14155, #13137, #7850, #1897 ) ) ;
#18195 = ORIENTED_EDGE ( 'NONE', *, *, #6343, .T. ) ;
#18196 = CARTESIAN_POINT ( 'NONE',  ( 6.761578195034432248, 37.80487342938723572, 78.00072712051441215 ) ) ;
#18197 = DIRECTION ( 'NONE',  ( 0.9480563259966798828, 0.3181025035074024343, 2.030702297275143506E-16 ) ) ;
#18198 = CARTESIAN_POINT ( 'NONE',  ( 5.451031912548643277, 50.71558463665398619, 77.95462253026452970 ) ) ;
#18199 = ORIENTED_EDGE ( 'NONE', *, *, #9485, .T. ) ;
#18200 = CARTESIAN_POINT ( 'NONE',  ( -4.398802922602397913, 51.46161812541917868, 78.75145056212190298 ) ) ;
#18201 = CARTESIAN_POINT ( 'NONE',  ( -4.158578283022523081, 37.42937009194850617, 76.53375056423675460 ) ) ;
#18202 = EDGE_LOOP ( 'NONE', ( #20200, #6102, #6873, #11172 ) ) ;
#18203 = CARTESIAN_POINT ( 'NONE',  ( 5.611423337425062385, 41.22389019960463230, 92.67996380123798872 ) ) ;
#18204 = EDGE_CURVE ( 'NONE', #12799, #9648, #14035, .T. ) ;
#18205 = CARTESIAN_POINT ( 'NONE',  ( 1.770248540159448103, 52.94298469573600130, 76.95808337915808295 ) ) ;
#18206 = EDGE_CURVE ( 'NONE', #5478, #14218, #5138, .T. ) ;
#18207 = CARTESIAN_POINT ( 'NONE',  ( -2.416137431568557314, 39.07291177436112406, 94.86746380123797451 ) ) ;
#18208 = B_SPLINE_SURFACE_WITH_KNOTS ( 'NONE', 3, 1, ( 
 ( #15852, #10974 ),
 ( #7760, #1267 ),
 ( #17445, #12550 ),
 ( #6050, #19041 ),
 ( #4453, #5031 ),
 ( #247, #18134 ),
 ( #3555, #11657 ),
 ( #5137, #16752 ),
 ( #11550, #18026 ),
 ( #2066, #3447 ),
 ( #10059, #16539 ),
 ( #6843, #13349 ),
 ( #11858, #5457 ),
 ( #19820, #9960 ),
 ( #13547, #565 ),
 ( #5242, #20023 ),
 ( #11758, #7048 ),
 ( #3862, #6943 ),
 ( #8563, #18232 ) ),
 .UNSPECIFIED., .F., .F., .F.,
 ( 4, 1, 1, 1, 1, 1, 1, 1, 1, 1, 1, 1, 1, 1, 1, 1, 4 ),
 ( 2, 2 ),
 ( 0.000000000000000000, 0.06114104454794499349, 0.1175581266966176375, 0.1702703359127188676, 0.2207833336891595610, 0.2680835234284920654, 0.3093802502289375589, 0.3470663877653532570, 0.3827844710311357757, 0.4080409699193555118, 0.4487658506906452294, 0.5030388115584650821, 0.5728007717267906695, 0.6580545229227713344, 0.7568648491070055773, 0.8711692811930628055, 1.000000000000000000 ),
 ( 0.000000000000000000, 1.000000000000000000 ),
 .UNSPECIFIED. ) ;
#18209 = LINE ( 'NONE', #19897, #19084 ) ;
#18210 = ORIENTED_EDGE ( 'NONE', *, *, #13656, .F. ) ;
#18211 = EDGE_CURVE ( 'NONE', #3672, #19886, #7862, .T. ) ;
#18212 = CARTESIAN_POINT ( 'NONE',  ( 4.393996117251955269, 36.11308595931626542, 76.96022115247204454 ) ) ;
#18213 = EDGE_CURVE ( 'NONE', #5759, #16046, #20824, .T. ) ;
#18214 = ORIENTED_EDGE ( 'NONE', *, *, #1162, .F. ) ;
#18215 = CARTESIAN_POINT ( 'NONE',  ( 27.03948732994508930, 45.16218137147969003, 76.90433879953101837 ) ) ;
#18216 = CARTESIAN_POINT ( 'NONE',  ( -0.3080929418689875576, 37.85583172076933778, 94.94558880123797451 ) ) ;
#18217 = ORIENTED_EDGE ( 'NONE', *, *, #4422, .F. ) ;
#18218 = LINE ( 'NONE', #1942, #10664 ) ;
#18219 = CARTESIAN_POINT ( 'NONE',  ( 8.159484030927535159, 41.62940053041398158, 75.36031793586835192 ) ) ;
#18220 = DIRECTION ( 'NONE',  ( 5.626130192357176673E-16, 1.831515347669941892E-30, -1.000000000000000000 ) ) ;
#18221 = AXIS2_PLACEMENT_3D ( 'NONE', #4888, #3615, #14690 ) ;
#18222 = CARTESIAN_POINT ( 'NONE',  ( -4.388990501910972952, 51.46862972198961472, 78.65149807507090429 ) ) ;
#18223 = CARTESIAN_POINT ( 'NONE',  ( 0.3328907573102549700, 52.96757149581038249, 78.56344688395670062 ) ) ;
#18224 = VERTEX_POINT ( 'NONE', #9364 ) ;
#18225 = CARTESIAN_POINT ( 'NONE',  ( -4.385532207686900996, 51.47110089242590902, 76.31459635612003467 ) ) ;
#18226 = ORIENTED_EDGE ( 'NONE', *, *, #16564, .T. ) ;
#18227 = DIRECTION ( 'NONE',  ( 0.3165065846431827645, 0.9485903129789529098, 0.000000000000000000 ) ) ;
#18228 = DIRECTION ( 'NONE',  ( 1.110223024625156540E-16, 1.000000000000000000, 5.922860397471808077E-17 ) ) ;
#18229 = LINE ( 'NONE', #14827, #6442 ) ;
#18230 = CARTESIAN_POINT ( 'NONE',  ( -4.884656273474450749, 44.39824779480852612, 93.03246379611699979 ) ) ;
#18231 = CARTESIAN_POINT ( 'NONE',  ( 4.666303754810079418, 40.22630141247467606, 95.46859283304921462 ) ) ;
#18232 = CARTESIAN_POINT ( 'NONE',  ( 5.495636600878563982, 37.64719334750368063, 76.58742703482498371 ) ) ;
#18233 = VECTOR ( 'NONE', #13965, 1000.000000000000000 ) ;
#18234 = VERTEX_POINT ( 'NONE', #4551 ) ;
#18235 = ADVANCED_FACE ( 'NONE', ( #9265 ), #12753, .T. ) ;
#18236 = CARTESIAN_POINT ( 'NONE',  ( 8.296628936784257391, 41.55497301399228149, 78.93669174070734584 ) ) ;
#18237 = CARTESIAN_POINT ( 'NONE',  ( 5.746684213116473039, 37.07966734754892713, 78.33482135361461474 ) ) ;
#18238 = ORIENTED_EDGE ( 'NONE', *, *, #6776, .T. ) ;
#18239 = LINE ( 'NONE', #469, #2041 ) ;
#18240 = CARTESIAN_POINT ( 'NONE',  ( -1.219503646467433144, 49.90383875825363447, 85.41268141275706682 ) ) ;
#18241 = CARTESIAN_POINT ( 'NONE',  ( 3.122153740306552905, 48.66551347115873227, 96.03933879953099506 ) ) ;
#18242 = ORIENTED_EDGE ( 'NONE', *, *, #1486, .T. ) ;
#18243 = CARTESIAN_POINT ( 'NONE',  ( 8.946756316568102108, 41.60772075457913388, 78.11862058389174024 ) ) ;
#18244 = CARTESIAN_POINT ( 'NONE',  ( -4.948764291328629383, 37.26291353443464516, 75.36972643424059015 ) ) ;
#18245 = ORIENTED_EDGE ( 'NONE', *, *, #4287, .F. ) ;
#18246 = CARTESIAN_POINT ( 'NONE',  ( 2.263811127080455954, 49.90383875825364157, 53.41268141275705972 ) ) ;
#18247 = DIRECTION ( 'NONE',  ( -1.334402673828313832E-16, 2.891205793294680792E-16, 1.000000000000000000 ) ) ;
#18248 = CARTESIAN_POINT ( 'NONE',  ( -0.2125050281363792815, 38.58189400963055959, 91.74246379953099506 ) ) ;
#18249 = ORIENTED_EDGE ( 'NONE', *, *, #652, .T. ) ;
#18250 = CARTESIAN_POINT ( 'NONE',  ( -4.517974409599093910, 36.94470640207592993, 78.25995115514949418 ) ) ;
#18251 = CARTESIAN_POINT ( 'NONE',  ( -5.154188915835984375, 42.64120994080404614, 96.11746380123797451 ) ) ;
#18252 = ORIENTED_EDGE ( 'NONE', *, *, #4434, .T. ) ;
#18253 = CARTESIAN_POINT ( 'NONE',  ( 0.6087969908866583957, 52.36175308762906155, 77.38466870788910512 ) ) ;
#18254 = CARTESIAN_POINT ( 'NONE',  ( 0.5981602388297567741, 52.96185312741366857, 75.36022115247205022 ) ) ;
#18255 =( NAMED_UNIT ( * ) PLANE_ANGLE_UNIT ( ) SI_UNIT ( $, .RADIAN. ) );
#18256 = CARTESIAN_POINT ( 'NONE',  ( 5.513055384645696222, 50.66842935564089601, 77.25219493245084834 ) ) ;
#18257 = CARTESIAN_POINT ( 'NONE',  ( 2.522153740306507519, 49.81903562097208038, 69.15433879953098995 ) ) ;
#18258 = ORIENTED_EDGE ( 'NONE', *, *, #12839, .T. ) ;
#18259 = ORIENTED_EDGE ( 'NONE', *, *, #287, .F. ) ;
#18260 = CARTESIAN_POINT ( 'NONE',  ( 4.958128353061608706, 36.51619420082643330, 75.49492869865662215 ) ) ;
#18261 = CARTESIAN_POINT ( 'NONE',  ( 7.705087751586725098, 40.25077934585792860, 78.89537297773202340 ) ) ;
#18262 = VECTOR ( 'NONE', #16821, 999.9999999999998863 ) ;
#18263 = EDGE_LOOP ( 'NONE', ( #2253, #6967 ) ) ;
#18264 = DIRECTION ( 'NONE',  ( 1.540237394707284220E-16, 1.793354297423764243E-16, -1.000000000000000000 ) ) ;
#18265 = FACE_OUTER_BOUND ( 'NONE', #3720, .T. ) ;
#18266 = CARTESIAN_POINT ( 'NONE',  ( -5.784195910403845176, 44.99242805365518194, 93.53933880123797451 ) ) ;
#18267 = ORIENTED_EDGE ( 'NONE', *, *, #10062, .T. ) ;
#18268 = EDGE_LOOP ( 'NONE', ( #14859, #14593 ) ) ;
#18269 = CARTESIAN_POINT ( 'NONE',  ( 6.811311454328823345, 50.45704851585021800, 79.04700635913849283 ) ) ;
#18270 = ORIENTED_EDGE ( 'NONE', *, *, #18796, .F. ) ;
#18271 = CARTESIAN_POINT ( 'NONE',  ( 5.507916691552521726, 50.67237191677704544, 76.01238189972890780 ) ) ;
#18272 = EDGE_CURVE ( 'NONE', #4403, #3928, #20441, .T. ) ;
#18273 = VECTOR ( 'NONE', #11986, 1000.000000000000000 ) ;
#18274 = DIRECTION ( 'NONE',  ( 1.000000000000000000, 0.000000000000000000, 0.000000000000000000 ) ) ;
#18275 = CARTESIAN_POINT ( 'NONE',  ( 4.113283266163863416, 51.52514030825627600, 77.01204236660041147 ) ) ;
#18276 = CARTESIAN_POINT ( 'NONE',  ( 8.377962481724168242, 41.81109640710783282, 77.32528637492231383 ) ) ;
#18277 = DIRECTION ( 'NONE',  ( 1.000000000000000000, 0.000000000000000000, 0.000000000000000000 ) ) ;
#18278 = CARTESIAN_POINT ( 'NONE',  ( 8.230998048249997368, 41.38260349656003001, 76.04813117819971069 ) ) ;
#18279 = CARTESIAN_POINT ( 'NONE',  ( 0.3016330202435082986, 38.27734481069801831, 92.55433879953096721 ) ) ;
#18280 = FACE_OUTER_BOUND ( 'NONE', #20718, .T. ) ;
#18281 = CARTESIAN_POINT ( 'NONE',  ( 6.828503391016846891, 43.33193468930419101, 94.00808880123798872 ) ) ;
#18282 = DIRECTION ( 'NONE',  ( 1.402518428993854849E-16, -1.000000000000000000, -1.734723475976787531E-14 ) ) ;
#18283 = ORIENTED_EDGE ( 'NONE', *, *, #9687, .F. ) ;
#18284 = CARTESIAN_POINT ( 'NONE',  ( 4.984017504316113900, 37.27956383785731731, 75.37664775417469798 ) ) ;
#18285 = CIRCLE ( 'NONE', #16939, 8.199999999999995737 ) ;
#18286 = EDGE_LOOP ( 'NONE', ( #16011, #16402, #232, #15181 ) ) ;
#18287 = CARTESIAN_POINT ( 'NONE',  ( 5.398882651910504649, 50.75441279359508684, 77.28963291717792572 ) ) ;
#18288 = CARTESIAN_POINT ( 'NONE',  ( 10.77494014480653561, 42.96218137147968008, 69.40574467885102194 ) ) ;
#18289 = CARTESIAN_POINT ( 'NONE',  ( 5.374105918413365046, 50.77268445065888613, 78.93541288588724569 ) ) ;
#18290 = CARTESIAN_POINT ( 'NONE',  ( 5.025485839985549319, 41.56218137147963887, 90.72683879953099506 ) ) ;
#18291 = CARTESIAN_POINT ( 'NONE',  ( -4.808920012916950704, 37.15961619924308934, 75.98775578934684916 ) ) ;
#18292 = DIRECTION ( 'NONE',  ( -1.000000000000000000, 0.000000000000000000, 0.000000000000000000 ) ) ;
#18293 = EDGE_CURVE ( 'NONE', #20173, #2871, #15750, .T. ) ;
#18294 = CARTESIAN_POINT ( 'NONE',  ( 5.902048492000326441, 51.12868443877599134, 78.27786821129558348 ) ) ;
#18295 = VERTEX_POINT ( 'NONE', #2862 ) ;
#18296 = EDGE_CURVE ( 'NONE', #9780, #6140, #19231, .T. ) ;
#18297 = CARTESIAN_POINT ( 'NONE',  ( 8.303614452336031349, 41.57589654819728509, 79.54845644658969661 ) ) ;
#18298 = PLANE ( 'NONE',  #14495 ) ;
#18299 = CARTESIAN_POINT ( 'NONE',  ( 1.855487073639843887, 49.49551470481303284, 53.82100546619766845 ) ) ;
#18300 = ORIENTED_EDGE ( 'NONE', *, *, #5094, .T. ) ;
#18301 = CARTESIAN_POINT ( 'NONE',  ( 2.722153740306497927, 50.36218137147968577, 37.95170767603170248 ) ) ;
#18302 = CIRCLE ( 'NONE', #2677, 8.199999999999995737 ) ;
#18303 = CARTESIAN_POINT ( 'NONE',  ( -4.588243132438923233, 36.99661107704094576, 78.89954634079194307 ) ) ;
#18304 = CARTESIAN_POINT ( 'NONE',  ( 5.544968037009670780, 45.50804040601273925, 92.44558880294498238 ) ) ;
#18305 = FACE_OUTER_BOUND ( 'NONE', #9288, .T. ) ;
#18306 = EDGE_CURVE ( 'NONE', #15079, #4532, #2652, .T. ) ;
#18307 = CARTESIAN_POINT ( 'NONE',  ( 5.568489401881125289, 48.03437091500646261, 90.57058880123798872 ) ) ;
#18308 = ADVANCED_FACE ( 'NONE', ( #7545 ), #2960, .F. ) ;
#18309 = CARTESIAN_POINT ( 'NONE',  ( -8.191743529290757664, 42.93415629907709530, 78.46397878055076092 ) ) ;
#18310 = EDGE_LOOP ( 'NONE', ( #19199, #16310, #594, #9107, #7173 ) ) ;
#18311 = CARTESIAN_POINT ( 'NONE',  ( 0.5221537403065010796, 44.16218137147969003, 45.55433879953098852 ) ) ;
#18312 = CIRCLE ( 'NONE', #15261, 8.799999999999995381 ) ;
#18313 = VERTEX_POINT ( 'NONE', #20518 ) ;
#18314 = CARTESIAN_POINT ( 'NONE',  ( -2.829262219629335551, 48.16467593588394891, 92.84494095006279224 ) ) ;
#18315 = EDGE_CURVE ( 'NONE', #2056, #2184, #5945, .T. ) ;
#18316 = CARTESIAN_POINT ( 'NONE',  ( 5.568489401881125289, 48.03437091500646261, 92.91433880123798872 ) ) ;
#18317 = ORIENTED_EDGE ( 'NONE', *, *, #13213, .F. ) ;
#18318 = ADVANCED_FACE ( 'NONE', ( #9889 ), #14763, .T. ) ;
#18319 = CARTESIAN_POINT ( 'NONE',  ( 8.302046940891129267, 41.57028864366792931, 78.04666919979170814 ) ) ;
#18320 = EDGE_CURVE ( 'NONE', #7787, #15579, #7006, .T. ) ;
#18322 = VECTOR ( 'NONE', #5505, 1000.000000000000000 ) ;
#18321 = CARTESIAN_POINT ( 'NONE',  ( 0.3821786226492927541, 35.36301154328572949, 76.16022115247204738 ) ) ;
#18323 = CARTESIAN_POINT ( 'NONE',  ( -3.713457647669470063, 51.95134076679423174, 79.29276450469329518 ) ) ;
#18324 = LINE ( 'NONE', #3741, #16729 ) ;
#18325 = ORIENTED_EDGE ( 'NONE', *, *, #2, .F. ) ;
#18326 = DIRECTION ( 'NONE',  ( 0.3165065846431826535, 0.9485903129789529098, 2.188653791613874008E-16 ) ) ;
#18327 = VECTOR ( 'NONE', #1863, 1000.000000000000000 ) ;
#18328 = EDGE_LOOP ( 'NONE', ( #6308, #16522, #7711, #14330, #162, #3118, #10936, #14004, #20791, #19568, #7578, #17313, #7971, #19712, #3588, #7624, #4216, #6930, #18423, #15013, #18697 ) ) ;
#18329 = PLANE ( 'NONE',  #18921 ) ;
#18330 = CARTESIAN_POINT ( 'NONE',  ( -7.022721810984192459, 41.30210581816755422, 76.72474157890661672 ) ) ;
#18331 = ADVANCED_FACE ( 'NONE', ( #8066 ), #11382, .F. ) ;
#18332 = VECTOR ( 'NONE', #2861, 1000.000000000000000 ) ;
#18333 = DIRECTION ( 'NONE',  ( -0.02533578529877749883, -0.9996789974703351733, -1.831801750099157288E-16 ) ) ;
#18334 = CARTESIAN_POINT ( 'NONE',  ( -7.290527651941959952, 40.11224193202943411, 78.50801527011910252 ) ) ;
#18335 = CARTESIAN_POINT ( 'NONE',  ( 2.463659247115865814, 38.82793883177424732, 95.37621379782397923 ) ) ;
#18336 = DIRECTION ( 'NONE',  ( -5.626130192357176673E-16, -1.831515347669941892E-30, 1.000000000000000000 ) ) ;
#18337 = AXIS2_PLACEMENT_3D ( 'NONE', #10746, #10642, #15621 ) ;
#18338 = VECTOR ( 'NONE', #1475, 1000.000000000000114 ) ;
#18339 = ORIENTED_EDGE ( 'NONE', *, *, #18926, .T. ) ;
#18340 = DIRECTION ( 'NONE',  ( -1.779391786395883536E-16, -5.922860397471806844E-17, 1.000000000000000000 ) ) ;
#18341 = DIRECTION ( 'NONE',  ( 1.000000000000000000, 5.595882180570345180E-16, 0.000000000000000000 ) ) ;
#18342 = EDGE_LOOP ( 'NONE', ( #12138, #15671, #11960, #11792 ) ) ;
#18343 = CARTESIAN_POINT ( 'NONE',  ( -2.825834663281994619, 48.16810349223129606, 93.78225227128625363 ) ) ;
#18344 = CARTESIAN_POINT ( 'NONE',  ( -3.943187491250720544, 40.73580453397070755, 94.08621379953100927 ) ) ;
#18345 = CARTESIAN_POINT ( 'NONE',  ( 4.987494971863720927, 47.58855820898865829, 92.21121379953100927 ) ) ;
#18346 = VECTOR ( 'NONE', #75, 1000.000000000000000 ) ;
#18347 = ORIENTED_EDGE ( 'NONE', *, *, #12013, .T. ) ;
#18348 = VECTOR ( 'NONE', #2278, 1000.000000000000000 ) ;
#18349 = CARTESIAN_POINT ( 'NONE',  ( 8.825683451842801119, 41.24485769827808213, 77.95380709400741637 ) ) ;
#18350 = DIRECTION ( 'NONE',  ( -0.5941461771851693774, -0.8043570849667760481, -2.357623395011396791E-16 ) ) ;
#18351 = EDGE_LOOP ( 'NONE', ( #5503, #8100, #17989, #17964 ) ) ;
#18352 = CARTESIAN_POINT ( 'NONE',  ( 5.567302800327750489, 36.95148795754280258, 75.36140480012781495 ) ) ;
#18353 = DIRECTION ( 'NONE',  ( 1.540237394707284220E-16, 1.793354297423764243E-16, -1.000000000000000000 ) ) ;
#18354 = ADVANCED_FACE ( 'NONE', ( #9683 ), #17852, .T. ) ;
#18355 = ORIENTED_EDGE ( 'NONE', *, *, #9011, .T. ) ;
#18356 = CARTESIAN_POINT ( 'NONE',  ( -4.275220640117388449, 37.54015509005341045, 77.94562699264550076 ) ) ;
#18357 = MECHANICAL_DESIGN_GEOMETRIC_PRESENTATION_REPRESENTATION (  '', ( #6456 ), #9886 ) ;
#18358 = ORIENTED_EDGE ( 'NONE', *, *, #873, .T. ) ;
#18359 = CARTESIAN_POINT ( 'NONE',  ( -4.739054262994943478, 51.21848697497132719, 76.01646854312687651 ) ) ;
#18360 = CARTESIAN_POINT ( 'NONE',  ( 2.722153740306499703, 47.73989013547934945, 45.55433879953098852 ) ) ;
#18361 = EDGE_CURVE ( 'NONE', #7434, #16241, #9782, .T. ) ;
#18362 = CARTESIAN_POINT ( 'NONE',  ( 6.828503391016846891, 43.33193468930419101, 91.50808880123798872 ) ) ;
#18363 = EDGE_CURVE ( 'NONE', #9648, #16344, #3373, .T. ) ;
#18364 = DIRECTION ( 'NONE',  ( 0.000000000000000000, 0.000000000000000000, 1.000000000000000000 ) ) ;
#18365 = CARTESIAN_POINT ( 'NONE',  ( -3.532917577324399261, 36.21708460058427193, 78.46683879953087626 ) ) ;
#18366 = AXIS2_PLACEMENT_3D ( 'NONE', #16153, #12647, #3061 ) ;
#18367 = CARTESIAN_POINT ( 'NONE',  ( 2.522153740306504854, 49.81903562097208038, 85.15433879953098995 ) ) ;
#18368 = CARTESIAN_POINT ( 'NONE',  ( 6.575359255040893913, 44.22010074469034180, 72.45432679953087529 ) ) ;
#18369 = VERTEX_POINT ( 'NONE', #12962 ) ;
#18370 = CARTESIAN_POINT ( 'NONE',  ( 4.410764955181007529, 36.12506835695402430, 76.35980278528342069 ) ) ;
#18371 = PRESENTATION_LAYER_ASSIGNMENT (  '', '', ( #15668 ) ) ;
#18372 = ORIENTED_EDGE ( 'NONE', *, *, #3343, .T. ) ;
#18373 = DIRECTION ( 'NONE',  ( 2.043266227890064411E-16, 0.7071067811865425767, -0.7071067811865524577 ) ) ;
#18374 = CARTESIAN_POINT ( 'NONE',  ( 0.3327559137711116333, 52.96757305357242984, 77.76169174070734869 ) ) ;
#18375 = CARTESIAN_POINT ( 'NONE',  ( -0.3080929418689875576, 37.85583172076933778, 95.10183880123796030 ) ) ;
#18376 = VERTEX_POINT ( 'NONE', #6352 ) ;
#18377 = ORIENTED_EDGE ( 'NONE', *, *, #20561, .T. ) ;
#18378 = LINE ( 'NONE', #16995, #3172 ) ;
#18379 = EDGE_LOOP ( 'NONE', ( #19738, #10365, #19412, #19012 ) ) ;
#18380 = DIRECTION ( 'NONE',  ( 1.000000000000000000, -0.000000000000000000, -0.000000000000000000 ) ) ;
#18381 = CARTESIAN_POINT ( 'NONE',  ( 0.5278000597222750612, 52.96709611985676247, 75.36134551364482093 ) ) ;
#18382 = DIRECTION ( 'NONE',  ( 0.5813877811927012917, -0.8136266022444372803, -5.636455622144620416E-17 ) ) ;
#18383 = CARTESIAN_POINT ( 'NONE',  ( -2.925772203269236371, 51.60219236238361873, 78.51222722775425211 ) ) ;
#18384 = CARTESIAN_POINT ( 'NONE',  ( 2.263811127080453733, 49.90383875825364157, 61.41268141275705972 ) ) ;
#18385 = CARTESIAN_POINT ( 'NONE',  ( 6.198496396448986090, 45.68315280215533392, 94.24246380123798872 ) ) ;
#18386 = PRODUCT ( 'Number Dial Wheels', 'Number Dial Wheels', '', ( #17094 ) ) ;
#18387 = CARTESIAN_POINT ( 'NONE',  ( 0.8348233090668778500, 52.35226028205824633, 77.59858114993788547 ) ) ;
#18388 = DIRECTION ( 'NONE',  ( -4.344610079045915326E-32, -6.093395702654244599E-48, -1.000000000000000000 ) ) ;
#18389 = CARTESIAN_POINT ( 'NONE',  ( 31.22215374030650281, 45.56218137147968861, 78.80433879953099563 ) ) ;
#18390 = CARTESIAN_POINT ( 'NONE',  ( 5.597054231160713655, 36.97274724074663510, 77.75916469768418438 ) ) ;
#18391 = CARTESIAN_POINT ( 'NONE',  ( -3.981178359372548492, 46.76218137147973408, 95.41433880294498238 ) ) ;
#18392 = AXIS2_PLACEMENT_3D ( 'NONE', #7881, #14150, #1714 ) ;
#18393 = CARTESIAN_POINT ( 'NONE',  ( -7.372922797599690270, 41.96044977055945679, 78.56636689789523587 ) ) ;
#18394 = EDGE_LOOP ( 'NONE', ( #19265, #4723, #3534, #3358 ) ) ;
#18395 = CARTESIAN_POINT ( 'NONE',  ( -4.537099264183358294, 37.70896829297682729, 76.38448585835440952 ) ) ;
#18396 = CIRCLE ( 'NONE', #9926, 4.200000000000000178 ) ;
#18397 = ORIENTED_EDGE ( 'NONE', *, *, #9125, .T. ) ;
#18398 = DIRECTION ( 'NONE',  ( 1.000000000000000000, 0.000000000000000000, 0.000000000000000000 ) ) ;
#18399 = CARTESIAN_POINT ( 'NONE',  ( 10.77494014480653561, 42.96218137147968008, 77.40433879953098995 ) ) ;
#18400 = CARTESIAN_POINT ( 'NONE',  ( 5.497743849324331578, 37.64424434608246628, 77.37492703482499223 ) ) ;
#18401 = CARTESIAN_POINT ( 'NONE',  ( -0.3080929418689875576, 37.85583172076933778, 95.10183880123796030 ) ) ;
#18402 = DIRECTION ( 'NONE',  ( 1.540237394707284220E-16, 1.793354297423764243E-16, -1.000000000000000000 ) ) ;
#18403 = DIRECTION ( 'NONE',  ( 0.000000000000000000, -1.000000000000000000, 0.000000000000000000 ) ) ;
#18404 = ADVANCED_FACE ( 'NONE', ( #11691 ), #14990, .T. ) ;
#18405 = CARTESIAN_POINT ( 'NONE',  ( 5.541713100162347416, 50.64173420093050026, 78.24916896818955081 ) ) ;
#18406 = VERTEX_POINT ( 'NONE', #6642 ) ;
#18407 = ORIENTED_EDGE ( 'NONE', *, *, #9128, .F. ) ;
#18408 = AXIS2_PLACEMENT_3D ( 'NONE', #820, #7305, #13794 ) ;
#18409 = FACE_OUTER_BOUND ( 'NONE', #465, .T. ) ;
#18410 = CARTESIAN_POINT ( 'NONE',  ( -4.537099264183358294, 37.70896829297682729, 77.05433879953086773 ) ) ;
#18411 = CARTESIAN_POINT ( 'NONE',  ( -5.590960105440975880, 48.67769231808699715, 75.45433879953087342 ) ) ;
#18412 = ORIENTED_EDGE ( 'NONE', *, *, #4669, .T. ) ;
#18413 = AXIS2_PLACEMENT_3D ( 'NONE', #4835, #6541, #3041 ) ;
#18414 = DIRECTION ( 'NONE',  ( 3.154042683594179442E-15, 4.423602989573997160E-31, -1.000000000000000000 ) ) ;
#18415 = CARTESIAN_POINT ( 'NONE',  ( 5.668901936282467524, 51.30090040776863702, 77.27261723006257910 ) ) ;
#18416 = DIRECTION ( 'NONE',  ( -5.626130192357176673E-16, -1.831515347669941892E-30, 1.000000000000000000 ) ) ;
#18417 = CARTESIAN_POINT ( 'NONE',  ( 6.102441102155617969, 43.42752260303680600, 89.86746380294499659 ) ) ;
#18418 = CARTESIAN_POINT ( 'NONE',  ( 1.567270154302307761, 52.94458525490427547, 76.85511030890285156 ) ) ;
#18419 = EDGE_CURVE ( 'NONE', #19622, #8316, #12936, .T. ) ;
#18420 = CARTESIAN_POINT ( 'NONE',  ( 2.043125170982144745, 38.48583871533720213, 91.42996380123798872 ) ) ;
#18421 = B_SPLINE_CURVE_WITH_KNOTS ( 'NONE', 3,
 ( #8056, #16251, #9671, #6338, #3363, #14752, #16150, #3266, #14543, #4951, #11576, #17839, #20907, #12951, #19431 ),
 .UNSPECIFIED., .F., .F.,
 ( 4, 1, 1, 1, 1, 1, 1, 1, 1, 1, 1, 1, 4 ),
 ( 0.000000000000000000, 0.1176523470896303353, 0.2161622001139844318, 0.3003057309359747351, 0.3785980537073788676, 0.4226998745584166772, 0.4746596431302817498, 0.5370400780653459272, 0.6084305140821594238, 0.6909958779695384301, 0.7839813792576545426, 0.8861497511813531958, 0.9999999999999998890 ),
 .UNSPECIFIED. ) ;
#18422 = CARTESIAN_POINT ( 'NONE',  ( -8.180775199338105708, 42.85845644839661617, 78.91515802863237639 ) ) ;
#18423 = ORIENTED_EDGE ( 'NONE', *, *, #4772, .F. ) ;
#18424 = AXIS2_PLACEMENT_3D ( 'NONE', #16271, #4655, #8075 ) ;
#18425 = CARTESIAN_POINT ( 'NONE',  ( 2.522153740306507963, 47.62628298661744708, 66.55433879953099563 ) ) ;
#18426 = ORIENTED_EDGE ( 'NONE', *, *, #1977, .T. ) ;
#18427 = CARTESIAN_POINT ( 'NONE',  ( 2.108290839596759447, 51.34989793853182505, 76.48963291717792856 ) ) ;
#18428 = CARTESIAN_POINT ( 'NONE',  ( -0.8237052942265477018, 49.18499566818285018, 95.25808880294498238 ) ) ;
#18429 = VERTEX_POINT ( 'NONE', #1659 ) ;
#18430 = LINE ( 'NONE', #16523, #9300 ) ;
#18431 = LINE ( 'NONE', #8548, #12529 ) ;
#18432 = ADVANCED_FACE ( 'NONE', ( #3350 ), #15926, .T. ) ;
#18433 = CARTESIAN_POINT ( 'NONE',  ( -2.914969352113478518, 51.60213568599777290, 78.15066919019970726 ) ) ;
#18434 = FACE_BOUND ( 'NONE', #20147, .T. ) ;
#18435 = CARTESIAN_POINT ( 'NONE',  ( 0.5221537403065008576, 44.16218137147968292, 80.45433879953087342 ) ) ;
#18436 = DIRECTION ( 'NONE',  ( -1.540237394707284220E-16, -1.793354297423764243E-16, 1.000000000000000000 ) ) ;
#18437 = ORIENTED_EDGE ( 'NONE', *, *, #17843, .F. ) ;
#18438 = CARTESIAN_POINT ( 'NONE',  ( 8.218856723678189979, 41.33361459021993767, 77.32290381395976908 ) ) ;
#18439 = CIRCLE ( 'NONE', #16064, 4.200000000000001954 ) ;
#18440 = ORIENTED_EDGE ( 'NONE', *, *, #7976, .T. ) ;
#18441 = LINE ( 'NONE', #13234, #20613 ) ;
#18442 = CIRCLE ( 'NONE', #17377, 0.9921021478795063464 ) ;
#18443 = CARTESIAN_POINT ( 'NONE',  ( 8.789147962602239517, 47.20595287382010241, 75.43669174070734584 ) ) ;
#18444 = EDGE_CURVE ( 'NONE', #9854, #16845, #11457, .T. ) ;
#18445 = CARTESIAN_POINT ( 'NONE',  ( 5.334770775912043739, 37.52292652420527475, 75.97297093591537021 ) ) ;
#18446 = CARTESIAN_POINT ( 'NONE',  ( 2.463659247115867590, 38.82793883177424732, 91.78246379782397923 ) ) ;
#18447 = CARTESIAN_POINT ( 'NONE',  ( 2.259191861956065139, 47.76843358786783966, 61.41730067788144964 ) ) ;
#18448 = ORIENTED_EDGE ( 'NONE', *, *, #18361, .T. ) ;
#18449 = CARTESIAN_POINT ( 'NONE',  ( 8.860816794629821302, 41.35015455542848173, 78.93613448519710118 ) ) ;
#18450 = EDGE_CURVE ( 'NONE', #10129, #970, #16343, .T. ) ;
#18451 = ORIENTED_EDGE ( 'NONE', *, *, #13105, .T. ) ;
#18452 = AXIS2_PLACEMENT_3D ( 'NONE', #13482, #4108, #8609 ) ;
#18453 = LINE ( 'NONE', #18557, #13938 ) ;
#18454 = CARTESIAN_POINT ( 'NONE',  ( -2.077846259693550746, 39.65884927180063357, 94.16433879953098085 ) ) ;
#18455 = CARTESIAN_POINT ( 'NONE',  ( -4.500660556396669065, 42.81632233694663370, 95.25808879953098085 ) ) ;
#18456 = ORIENTED_EDGE ( 'NONE', *, *, #12099, .F. ) ;
#18457 = DIRECTION ( 'NONE',  ( -0.5941461771851691553, -0.8043570849667760481, -2.357623395011396791E-16 ) ) ;
#18458 = PLANE ( 'NONE',  #7570 ) ;
#18459 = CARTESIAN_POINT ( 'NONE',  ( 2.475532831258718591, 39.44063218796383552, 95.05433879953096721 ) ) ;
#18460 = CARTESIAN_POINT ( 'NONE',  ( 8.951667845840693971, 41.62244091939069790, 78.41904468188381827 ) ) ;
#18461 = CARTESIAN_POINT ( 'NONE',  ( -2.904223097202481174, 48.62752260303690122, 91.27371379953098085 ) ) ;
#18462 = VERTEX_POINT ( 'NONE', #6227 ) ;
#18463 = CARTESIAN_POINT ( 'NONE',  ( -4.598246518171406727, 51.31910303412164609, 78.93669174070734584 ) ) ;
#18464 = CARTESIAN_POINT ( 'NONE',  ( 4.001624342216747010, 40.29782057951908314, 90.66473080991372058 ) ) ;
#18465 = ORIENTED_EDGE ( 'NONE', *, *, #3511, .T. ) ;
#18466 = CARTESIAN_POINT ( 'NONE',  ( -4.449507049815707660, 50.67847138028889020, 76.30694920102484957 ) ) ;
#18467 = FACE_OUTER_BOUND ( 'NONE', #2127, .T. ) ;
#18468 = CARTESIAN_POINT ( 'NONE',  ( 3.460444912181559474, 49.25145096859824889, 90.49246380123798872 ) ) ;
#18469 = VECTOR ( 'NONE', #11501, 1000.000000000000000 ) ;
#18470 = APPLICATION_PROTOCOL_DEFINITION ( 'draft international standard', 'automotive_design', 1998, #4361 ) ;
#18471 = CARTESIAN_POINT ( 'NONE',  ( -4.374766499958361976, 37.59356042999372960, 75.97251605650340878 ) ) ;
#18473 = ADVANCED_FACE ( 'NONE', ( #13146 ), #11355, .F. ) ;
#18472 = CARTESIAN_POINT ( 'NONE',  ( -3.955205046931956403, 36.52901134360649138, 77.68963291717793140 ) ) ;
#18474 = CARTESIAN_POINT ( 'NONE',  ( -4.157569799700691959, 37.42619470865965070, 79.54087410433339755 ) ) ;
#18475 = EDGE_CURVE ( 'NONE', #2806, #20010, #4621, .T. ) ;
#18476 = ORIENTED_EDGE ( 'NONE', *, *, #19772, .F. ) ;
#18477 = CARTESIAN_POINT ( 'NONE',  ( 1.885276772082373542, 52.95616720758849283, 75.75738117569228791 ) ) ;
#18478 = ORIENTED_EDGE ( 'NONE', *, *, #13643, .T. ) ;
#18479 = CARTESIAN_POINT ( 'NONE',  ( 31.07218010054375412, 42.96218137147968008, 65.80574467885102763 ) ) ;
#18480 = EDGE_CURVE ( 'NONE', #10614, #6705, #9820, .T. ) ;
#18481 = CARTESIAN_POINT ( 'NONE',  ( 0.3917809267179716559, 52.96710761965328373, 77.46088296688223807 ) ) ;
#18482 = CARTESIAN_POINT ( 'NONE',  ( -4.567115856812060670, 47.10047254335474065, 95.96121380123798872 ) ) ;
#18483 = VERTEX_POINT ( 'NONE', #12825 ) ;
#18484 = VERTEX_POINT ( 'NONE', #4721 ) ;
#18485 = ADVANCED_FACE ( 'NONE', ( #11250 ), #14456, .T. ) ;
#18486 = VECTOR ( 'NONE', #3214, 1000.000000000000114 ) ;
#18487 = CARTESIAN_POINT ( 'NONE',  ( 0.3279640439667347862, 52.35988168082469940, 76.44919174070734869 ) ) ;
#18488 = ORIENTED_EDGE ( 'NONE', *, *, #811, .T. ) ;
#18489 = EDGE_CURVE ( 'NONE', #2672, #16604, #18925, .T. ) ;
#18490 = CARTESIAN_POINT ( 'NONE',  ( 5.545031559531118148, 50.64376324557171216, 76.06405336652188964 ) ) ;
#18491 = PLANE ( 'NONE',  #14935 ) ;
#18492 = CARTESIAN_POINT ( 'NONE',  ( 7.857645200629401749, 40.72477040771212842, 75.53366564255911442 ) ) ;
#18493 = CARTESIAN_POINT ( 'NONE',  ( 5.282950423531485917, 37.48574407745871895, 77.76022115247205591 ) ) ;
#18494 = DIRECTION ( 'NONE',  ( -1.000000000000000000, 0.000000000000000000, 0.000000000000000000 ) ) ;
#18495 = CARTESIAN_POINT ( 'NONE',  ( 30.92220646078100188, 42.96218137147968008, 61.80715055817104542 ) ) ;
#18496 = CARTESIAN_POINT ( 'NONE',  ( -3.350035803220276609, 49.20851703305431357, 94.63308880123798872 ) ) ;
#18497 = CARTESIAN_POINT ( 'NONE',  ( 8.211374823828526459, 41.32379144809473104, 76.38644048143638088 ) ) ;
#18498 = CARTESIAN_POINT ( 'NONE',  ( -1.579458713458412822, 38.67424504376464967, 92.55433879953098142 ) ) ;
#18499 = DIRECTION ( 'NONE',  ( 1.779391786395883536E-16, 5.922860397471806844E-17, -1.000000000000000000 ) ) ;
#18500 = CARTESIAN_POINT ( 'NONE',  ( 5.544968037009670780, 45.50804040601273925, 93.69558880294498238 ) ) ;
#18501 = CARTESIAN_POINT ( 'NONE',  ( 8.306997239855295589, 41.58599280843245793, 75.97301370697266520 ) ) ;
#18502 = ORIENTED_EDGE ( 'NONE', *, *, #2302, .T. ) ;
#18503 = CARTESIAN_POINT ( 'NONE',  ( 0.5294070821904082180, 52.96600742907325099, 75.97350791242078571 ) ) ;
#18504 = EDGE_LOOP ( 'NONE', ( #322, #3984, #13378, #3462, #14713, #17572, #6674, #6502, #6398, #2301, #14693, #7407, #924, #8599, #18217, #1219, #5296, #128, #12418, #9736, #20014 ) ) ;
#18505 = CARTESIAN_POINT ( 'NONE',  ( -4.517072128342570991, 36.94403992325788977, 76.53375056423675460 ) ) ;
#18506 = CARTESIAN_POINT ( 'NONE',  ( -2.073200253767598866, 36.38374080505226971, 80.45433879953087342 ) ) ;
#18507 = ADVANCED_FACE ( 'NONE', ( #20717 ), #1264, .F. ) ;
#18508 = CARTESIAN_POINT ( 'NONE',  ( -4.394494991871735756, 50.72473661586263916, 78.89396334764496999 ) ) ;
#18509 = CARTESIAN_POINT ( 'NONE',  ( 6.828503391016846891, 43.33193468930419101, 92.91433880123798872 ) ) ;
#18510 = CARTESIAN_POINT ( 'NONE',  ( -4.735411308350331083, 37.10531828029096602, 75.97251605650340878 ) ) ;
#18511 = CARTESIAN_POINT ( 'NONE',  ( 0.5221537403065006355, 44.16218137147969003, 92.45433879953097289 ) ) ;
#18512 = DIRECTION ( 'NONE',  ( -1.193617070626243484E-16, -1.000000000000000000, -0.000000000000000000 ) ) ;
#18513 = CARTESIAN_POINT ( 'NONE',  ( 5.901631269491789844, 51.12899262423628954, 78.24916896818955081 ) ) ;
#18514 = EDGE_LOOP ( 'NONE', ( #8799, #134, #5702, #16605 ) ) ;
#18515 = ORIENTED_EDGE ( 'NONE', *, *, #12353, .F. ) ;
#18516 = MANIFOLD_SOLID_BREP ( 'Stock-MAS-160-1', #14936 ) ;
#18517 = DIRECTION ( 'NONE',  ( -1.540237394707284220E-16, -1.793354297423764243E-16, 1.000000000000000000 ) ) ;
#18518 = DIRECTION ( 'NONE',  ( -0.9485903129789527988, 0.3165065846431829311, -8.934458285744989980E-17 ) ) ;
#18519 = DIRECTION ( 'NONE',  ( -5.626130192357176673E-16, -1.831515347669941892E-30, 1.000000000000000000 ) ) ;
#18520 = ORIENTED_EDGE ( 'NONE', *, *, #8796, .T. ) ;
#18521 = CARTESIAN_POINT ( 'NONE',  ( -4.652687709939232086, 51.28020135170361016, 75.36022115247205022 ) ) ;
#18522 = CARTESIAN_POINT ( 'NONE',  ( 6.012275498921958672, 37.26944915646792822, 78.37198585835440667 ) ) ;
#18523 = CARTESIAN_POINT ( 'NONE',  ( 9.353817388681445522, 42.82770861117572281, 77.06316232894263862 ) ) ;
#18524 = DIRECTION ( 'NONE',  ( -2.409338161078896715E-16, 1.000000000000000000, 0.000000000000000000 ) ) ;
#18525 = CARTESIAN_POINT ( 'NONE',  ( -7.333990156426536622, 40.19720935722482835, 76.16022115247204738 ) ) ;
#18526 = CARTESIAN_POINT ( 'NONE',  ( -6.983651697411273673, 47.33966115288628629, 78.30768265673681583 ) ) ;
#18527 = CARTESIAN_POINT ( 'NONE',  ( -0.9988176903691428077, 49.83852402762217082, 93.14871380123798872 ) ) ;
#18528 = CARTESIAN_POINT ( 'NONE',  ( -3.682072889308531494, 36.32725962120449026, 77.89282216559597316 ) ) ;
#18529 = LINE ( 'NONE', #19995, #7526 ) ;
#18530 = ORIENTED_EDGE ( 'NONE', *, *, #20533, .T. ) ;
#18531 = CARTESIAN_POINT ( 'NONE',  ( 2.114036233085143657, 52.20617982865869067, 76.39831061904099840 ) ) ;
#18532 = ORIENTED_EDGE ( 'NONE', *, *, #19884, .T. ) ;
#18533 = CARTESIAN_POINT ( 'NONE',  ( 1.514255888186008203, 51.36218137147968577, 52.53721119516358584 ) ) ;
#18534 = CARTESIAN_POINT ( 'NONE',  ( 1.868012774839550749, 39.13936707477651566, 94.63308880294498238 ) ) ;
#18535 = VERTEX_POINT ( 'NONE', #2764 ) ;
#18536 = CARTESIAN_POINT ( 'NONE',  ( 5.666884522201895535, 41.76315400873614436, 93.18871379782397923 ) ) ;
#18537 = DIRECTION ( 'NONE',  ( 1.000000000000000000, 0.000000000000000000, 0.000000000000000000 ) ) ;
#18538 = CARTESIAN_POINT ( 'NONE',  ( -3.278373844761569345, 51.34246014063911900, 79.29276450469329518 ) ) ;
#18539 = B_SPLINE_CURVE_WITH_KNOTS ( 'NONE', 3,
 ( #996, #7377, #12291, #10713, #3865, #13867, #4078, #18555, #17074, #10493, #12074, #8774, #9094, #20348 ),
 .UNSPECIFIED., .F., .F.,
 ( 4, 2, 2, 2, 2, 2, 4 ),
 ( 0.000000000000000000, 0.0001700352343923301106, 0.0003400704687846602212, 0.0005101057031769903318, 0.0006801409375693204425, 0.001020211406354016659, 0.001360281875138712876 ),
 .UNSPECIFIED. ) ;
#18540 = FACE_OUTER_BOUND ( 'NONE', #20058, .T. ) ;
#18541 = CARTESIAN_POINT ( 'NONE',  ( 0.8485110817020684593, 52.96358246935430714, 76.26682227151283655 ) ) ;
#18542 = CARTESIAN_POINT ( 'NONE',  ( 0.3467791549783648120, 52.96746198069069322, 78.72223189599347393 ) ) ;
#18543 = VERTEX_POINT ( 'NONE', #12659 ) ;
#18544 = FACE_OUTER_BOUND ( 'NONE', #3330, .T. ) ;
#18545 = EDGE_CURVE ( 'NONE', #9005, #1116, #15752, .T. ) ;
#18546 = ORIENTED_EDGE ( 'NONE', *, *, #1842, .T. ) ;
#18547 = CARTESIAN_POINT ( 'NONE',  ( 6.489847418355314979, 49.78593742637539776, 78.48669174070734300 ) ) ;
#18548 = CARTESIAN_POINT ( 'NONE',  ( 4.143017335158133641, 51.51944627275094746, 78.46169174070733732 ) ) ;
#18549 = CARTESIAN_POINT ( 'NONE',  ( 6.949446517235058352, 50.35501370930113296, 76.97234655072247733 ) ) ;
#18550 = CARTESIAN_POINT ( 'NONE',  ( 5.495005229380907963, 37.64215342952340393, 76.33323713518528564 ) ) ;
#18551 = CARTESIAN_POINT ( 'NONE',  ( 2.921181103050039418, 49.30691215337508737, 92.25121379782397923 ) ) ;
#18552 = CARTESIAN_POINT ( 'NONE',  ( -1.677846259693499542, 50.36218137147968577, 54.55433879953098852 ) ) ;
#18553 = EDGE_CURVE ( 'NONE', #12696, #13249, #17440, .T. ) ;
#18554 = VERTEX_POINT ( 'NONE', #20827 ) ;
#18555 = CARTESIAN_POINT ( 'NONE',  ( 4.206193916732119398, 51.48810741143868341, 77.38277586711910772 ) ) ;
#18556 = VERTEX_POINT ( 'NONE', #17126 ) ;
#18557 = CARTESIAN_POINT ( 'NONE',  ( 1.771153339986190067, 40.36218137147969998, 45.55433879953100273 ) ) ;
#18558 = CARTESIAN_POINT ( 'NONE',  ( 3.122153740306552905, 48.66551347115873227, 93.53933879953099506 ) ) ;
#18559 = CARTESIAN_POINT ( 'NONE',  ( 1.868012774839550749, 39.13936707477651566, 95.57058879953099506 ) ) ;
#18560 = B_SPLINE_SURFACE_WITH_KNOTS ( 'NONE', 3, 1, ( 
 ( #12591, #20757 ),
 ( #19483, #11110 ),
 ( #17577, #19380 ),
 ( #4898, #3113 ),
 ( #19080, #9615 ),
 ( #4490, #8005 ),
 ( #11010, #1520 ),
 ( #2907, #837 ),
 ( #8215, #15318 ),
 ( #10539, #13603 ),
 ( #11807, #3814 ),
 ( #125, #2439 ),
 ( #18393, #6990 ),
 ( #13110, #5722 ),
 ( #12027, #8935 ) ),
 .UNSPECIFIED., .F., .F., .F.,
 ( 4, 1, 1, 1, 1, 1, 1, 1, 1, 1, 1, 1, 4 ),
 ( 2, 2 ),
 ( 0.000000000000000000, 0.1147061202499928684, 0.2167524336893861536, 0.3108875303107388466, 0.4039803747164272818, 0.4534531356382086598, 0.5079179071285299107, 0.5705472921755296856, 0.6391587557001583431, 0.7163993029626264386, 0.8030541331324966281, 0.8966574343170833350, 1.000000000000000000 ),
 ( 0.000000000000000000, 1.000000000000000000 ),
 .UNSPECIFIED. ) ;
#18561 = VERTEX_POINT ( 'NONE', #2549 ) ;
#18562 = CARTESIAN_POINT ( 'NONE',  ( -4.524181921268124462, 40.28999182795290324, 93.69558880123800293 ) ) ;
#18563 = DIRECTION ( 'NONE',  ( 0.3165065846431827645, 0.9485903129789529098, 0.000000000000000000 ) ) ;
#18564 = EDGE_LOOP ( 'NONE', ( #13317, #392, #13678, #577 ) ) ;
#18565 = LINE ( 'NONE', #2186, #18273 ) ;
#18566 = FACE_BOUND ( 'NONE', #4770, .T. ) ;
#18567 = EDGE_LOOP ( 'NONE', ( #11584, #12303, #744, #19985 ) ) ;
#18568 = CARTESIAN_POINT ( 'NONE',  ( 0.6404851603139647409, 52.36132752672286017, 79.54845644658969661 ) ) ;
#18569 = CARTESIAN_POINT ( 'NONE',  ( -2.416137431568557314, 39.07291177436112406, 96.27371380123797451 ) ) ;
#18570 = EDGE_CURVE ( 'NONE', #15771, #4901, #9045, .T. ) ;
#18571 = EDGE_LOOP ( 'NONE', ( #19652, #11668, #10684, #18440 ) ) ;
#18572 = CARTESIAN_POINT ( 'NONE',  ( -4.408955773324692018, 50.70744783779237963, 76.05031124229590489 ) ) ;
#18573 = DIRECTION ( 'NONE',  ( -1.402518428993831676E-16, 1.000000000000000000, -0.000000000000000000 ) ) ;
#18574 = AXIS2_PLACEMENT_3D ( 'NONE', #4555, #7763, #17134 ) ;
#18575 = FACE_OUTER_BOUND ( 'NONE', #1673, .T. ) ;
#18576 = PRODUCT_RELATED_PRODUCT_CATEGORY ( 'part', '', ( #13807 ) ) ;
#18577 = DIRECTION ( 'NONE',  ( -1.000000000000000000, 0.000000000000000000, 0.000000000000000000 ) ) ;
#18578 = CARTESIAN_POINT ( 'NONE',  ( 23.63948732994508006, 45.16218137147969003, 76.90433879953101837 ) ) ;
#18579 = EDGE_CURVE ( 'NONE', #6883, #14176, #5844, .T. ) ;
#18580 = CARTESIAN_POINT ( 'NONE',  ( 0.5981954327195757593, 52.96631631695955633, 75.36022115247205022 ) ) ;
#18581 = ADVANCED_FACE ( 'NONE', ( #21024 ), #1895, .F. ) ;
#18582 = ORIENTED_EDGE ( 'NONE', *, *, #7514, .T. ) ;
#18583 = CARTESIAN_POINT ( 'NONE',  ( 0.1632948971478923317, 52.35765006764384566, 79.53017257457305789 ) ) ;
#18584 = DIRECTION ( 'NONE',  ( 0.3165065846431827645, 0.9485903129789529098, 0.000000000000000000 ) ) ;
#18585 = CARTESIAN_POINT ( 'NONE',  ( 1.352400422481993658, 50.46853102219002096, 94.47683880123798872 ) ) ;
#18586 = ORIENTED_EDGE ( 'NONE', *, *, #1451, .F. ) ;
#18587 = AXIS2_PLACEMENT_3D ( 'NONE', #15565, #2162, #13966 ) ;
#18588 = EDGE_CURVE ( 'NONE', #6294, #6753, #19784, .T. ) ;
#18589 = CARTESIAN_POINT ( 'NONE',  ( 0.3821786226492926430, 35.36301154328572949, 76.86610350541323555 ) ) ;
#18590 = EDGE_LOOP ( 'NONE', ( #5921, #20098, #14214, #19218 ) ) ;
#18591 = DIRECTION ( 'NONE',  ( -1.540237394707284467E-16, -1.793354297423764243E-16, 1.000000000000000000 ) ) ;
#18592 = ADVANCED_FACE ( 'NONE', ( #1483 ), #8894, .T. ) ;
#18593 = FACE_OUTER_BOUND ( 'NONE', #4337, .T. ) ;
#18594 = CARTESIAN_POINT ( 'NONE',  ( -2.313335635445064931, 37.76218137147968434, 95.05433879953096721 ) ) ;
#18596 = ADVANCED_FACE ( 'NONE', ( #8172 ), #8283, .T. ) ;
#18595 = CARTESIAN_POINT ( 'NONE',  ( -4.058243788015966302, 50.96439249353348089, 79.54394747197609661 ) ) ;
#18597 = DIRECTION ( 'NONE',  ( -1.000000000000000000, -1.402518428993809490E-16, 6.308085367188358884E-15 ) ) ;
#18598 = FACE_OUTER_BOUND ( 'NONE', #12569, .T. ) ;
#18599 = CARTESIAN_POINT ( 'NONE',  ( 0.6318382202979666573, 52.35386089408143562, 77.38563349023446847 ) ) ;
#18600 = CARTESIAN_POINT ( 'NONE',  ( 11.22215374030650281, 42.96218137147968008, 58.20715055817105110 ) ) ;
#18601 = CARTESIAN_POINT ( 'NONE',  ( 1.868012774839550749, 39.13936707477651566, 94.63308880294498238 ) ) ;
#18602 = EDGE_CURVE ( 'NONE', #16595, #7376, #1188, .T. ) ;
#18603 = CARTESIAN_POINT ( 'NONE',  ( -3.981178359372548492, 46.76218137147973408, 91.66433880294496817 ) ) ;
#18604 = AXIS2_PLACEMENT_3D ( 'NONE', #15415, #8926, #11799 ) ;
#18605 = CARTESIAN_POINT ( 'NONE',  ( -0.8111795930268257404, 49.49551470481303284, 69.82100546619766135 ) ) ;
#18606 = CARTESIAN_POINT ( 'NONE',  ( 8.370524243984743151, 41.80079226538762072, 78.80177617112552468 ) ) ;
#18607 = ORIENTED_EDGE ( 'NONE', *, *, #8741, .T. ) ;
#18608 = CARTESIAN_POINT ( 'NONE',  ( 30.43948732994507722, 43.16218137147969003, 74.70433879953098710 ) ) ;
#18609 = CARTESIAN_POINT ( 'NONE',  ( 0.5221537403065019678, 51.36218137147968577, 48.36106904222365444 ) ) ;
#18610 = CARTESIAN_POINT ( 'NONE',  ( -4.524181921268124462, 40.28999182795290324, 93.69558880123800293 ) ) ;
#18611 = VECTOR ( 'NONE', #9584, 1000.000000000000000 ) ;
#18612 = CARTESIAN_POINT ( 'NONE',  ( -4.894326847483570830, 37.22270278754029960, 76.26481528174605273 ) ) ;
#18613 = CARTESIAN_POINT ( 'NONE',  ( -6.926305133125032043, 47.45453072168001540, 78.88364539996459257 ) ) ;
#18614 = DIRECTION ( 'NONE',  ( 0.007885122365275663500, 0.9999689119394085113, 1.805443505845543142E-16 ) ) ;
#18615 = CARTESIAN_POINT ( 'NONE',  ( 5.401236444110097956, 50.74549864801142718, 77.94923276678728996 ) ) ;
#18616 = VERTEX_POINT ( 'NONE', #16474 ) ;
#18617 = VERTEX_POINT ( 'NONE', #14866 ) ;
#18618 = VECTOR ( 'NONE', #18698, 1000.000000000000227 ) ;
#18619 = CARTESIAN_POINT ( 'NONE',  ( 8.514005641241574551, 42.67515757794754450, 79.29919401074631935 ) ) ;
#18621 = EDGE_CURVE ( 'NONE', #15492, #3149, #12981, .T. ) ;
#18620 = CARTESIAN_POINT ( 'NONE',  ( -1.477846259693490261, 47.62628298661744708, 45.55433879953100273 ) ) ;
#18622 = CARTESIAN_POINT ( 'NONE',  ( -1.677846259693499542, 44.16218137147969003, 54.55433879953098852 ) ) ;
#18623 = CARTESIAN_POINT ( 'NONE',  ( -5.368445182934982185, 36.96218137147968008, 95.05433879953098142 ) ) ;
#18624 = CARTESIAN_POINT ( 'NONE',  ( 5.605180980092264953, 51.34796851126965578, 77.21343514867072599 ) ) ;
#18625 = DIRECTION ( 'NONE',  ( 1.110223024625156540E-16, 1.000000000000000000, 5.922860397471808077E-17 ) ) ;
#18626 = CARTESIAN_POINT ( 'NONE',  ( -0.8237052942265477018, 49.18499566818285018, 90.25808880294496817 ) ) ;
#18627 = EDGE_CURVE ( 'NONE', #19487, #20830, #600, .T. ) ;
#18628 = AXIS2_PLACEMENT_3D ( 'NONE', #5663, #7479, #2378 ) ;
#18629 = CARTESIAN_POINT ( 'NONE',  ( 0.5221537403065114047, 44.16218137147969713, 45.55433879953100273 ) ) ;
#18630 = CARTESIAN_POINT ( 'NONE',  ( -7.016843279332989347, 47.24018387623220150, 78.28954034321952804 ) ) ;
#18631 = CARTESIAN_POINT ( 'NONE',  ( 0.5221537403065014127, 44.16218137147968292, 76.48963291717792856 ) ) ;
#18632 = DIRECTION ( 'NONE',  ( -1.540237394707284220E-16, -1.793354297423764243E-16, 1.000000000000000000 ) ) ;
#18633 = CARTESIAN_POINT ( 'NONE',  ( 5.826095025493096990, 51.18478820489261949, 78.92065061514911406 ) ) ;
#18634 = CARTESIAN_POINT ( 'NONE',  ( -1.219503646467430036, 49.90383875825363447, 69.41268141275705261 ) ) ;
#18635 = ORIENTED_EDGE ( 'NONE', *, *, #13374, .T. ) ;
#18636 = FACE_OUTER_BOUND ( 'NONE', #15611, .T. ) ;
#18637 = CARTESIAN_POINT ( 'NONE',  ( -3.350035803220276609, 49.20851703305431357, 93.22683880123798872 ) ) ;
#18638 = VERTEX_POINT ( 'NONE', #6774 ) ;
#18639 = CARTESIAN_POINT ( 'NONE',  ( 2.463659247115867146, 38.82793883177424732, 93.03246379782397923 ) ) ;
#18640 = VECTOR ( 'NONE', #7580, 1000.000000000000000 ) ;
#18641 = CARTESIAN_POINT ( 'NONE',  ( -1.187946976321872850, 48.86064447540922373, 94.36058879953097289 ) ) ;
#18642 = CARTESIAN_POINT ( 'NONE',  ( -3.838985764043254090, 50.94186738843281859, 79.52610421797659512 ) ) ;
#18643 = PLANE ( 'NONE',  #1288 ) ;
#18644 = CARTESIAN_POINT ( 'NONE',  ( 5.561792858816290597, 51.38001756867608094, 76.94115191089467487 ) ) ;
#18645 = CARTESIAN_POINT ( 'NONE',  ( -3.096104608208455122, 36.80844346142616530, 78.46683879953087626 ) ) ;
#18646 = ORIENTED_EDGE ( 'NONE', *, *, #5529, .T. ) ;
#18647 = DIRECTION ( 'NONE',  ( -1.540237394707284220E-16, -1.793354297423764243E-16, 1.000000000000000000 ) ) ;
#18648 = EDGE_LOOP ( 'NONE', ( #9344, #1354, #4569, #7216 ) ) ;
#18649 = CARTESIAN_POINT ( 'NONE',  ( 4.668718747243733702, 52.03969543967511413, 77.44183710417100031 ) ) ;
#18650 = CARTESIAN_POINT ( 'NONE',  ( 25.63948732994507651, 43.16218137147969003, 74.70433879953100131 ) ) ;
#18651 = FACE_OUTER_BOUND ( 'NONE', #14007, .T. ) ;
#18652 = CARTESIAN_POINT ( 'NONE',  ( -7.527492150214135869, 40.60566315307306695, 77.34111263368903622 ) ) ;
#18653 = CARTESIAN_POINT ( 'NONE',  ( 28.52215374030649997, 44.16218137147968292, 87.05433879953099563 ) ) ;
#18654 = CARTESIAN_POINT ( 'NONE',  ( -4.812088799398940075, 42.22067586467031930, 93.96996379782397923 ) ) ;
#18655 = LINE ( 'NONE', #12391, #18080 ) ;
#18656 = AXIS2_PLACEMENT_3D ( 'NONE', #18116, #16521, #1939 ) ;
#18657 = EDGE_LOOP ( 'NONE', ( #18586, #11319, #20166, #2026, #11024, #8249 ) ) ;
#18658 = DIRECTION ( 'NONE',  ( 0.5813877811927011807, -0.8136266022444372803, -5.636455622144619183E-17 ) ) ;
#18659 = ORIENTED_EDGE ( 'NONE', *, *, #7927, .F. ) ;
#18660 = CARTESIAN_POINT ( 'NONE',  ( 28.52215374030650352, 44.16218137147969003, 105.5543387995309956 ) ) ;
#18661 = CARTESIAN_POINT ( 'NONE',  ( -2.904223097202481174, 48.62752260303690122, 92.52371379953099506 ) ) ;
#18662 = ORIENTED_EDGE ( 'NONE', *, *, #11160, .T. ) ;
#18663 = CARTESIAN_POINT ( 'NONE',  ( -4.567115856812060670, 47.10047254335474065, 93.46121380123797451 ) ) ;
#18664 = CARTESIAN_POINT ( 'NONE',  ( 5.856396280011939126, 46.10368687828906076, 94.43871379782397923 ) ) ;
#18665 = CARTESIAN_POINT ( 'NONE',  ( 2.115041367457929589, 52.20598078514408513, 77.84551527011910821 ) ) ;
#18666 = DIRECTION ( 'NONE',  ( -1.540237394707284220E-16, -1.793354297423764243E-16, 1.000000000000000000 ) ) ;
#18667 = CARTESIAN_POINT ( 'NONE',  ( -4.766891056059167298, 51.19859582181767621, 78.86176377286571437 ) ) ;
#18668 = ORIENTED_EDGE ( 'NONE', *, *, #19975, .T. ) ;
#18669 = DIRECTION ( 'NONE',  ( 0.007885122365275663500, 0.9999689119394085113, 1.805443505845543142E-16 ) ) ;
#18670 = VECTOR ( 'NONE', #19853, 1000.000000000000000 ) ;
#18671 = CARTESIAN_POINT ( 'NONE',  ( 1.352400422481993658, 50.46853102219002096, 93.22683880123798872 ) ) ;
#18672 = ORIENTED_EDGE ( 'NONE', *, *, #10710, .T. ) ;
#18673 = CARTESIAN_POINT ( 'NONE',  ( -0.2740250116460755114, 39.09885644656073111, 92.45433879953098710 ) ) ;
#18674 = DIRECTION ( 'NONE',  ( -0.6080936526121348829, -0.7938652969193401576, -2.360290325043241294E-16 ) ) ;
#18675 =( BOUNDED_CURVE ( )  B_SPLINE_CURVE ( 2, ( #11178, #20624, #4656, #15962, #14463 ),
 .UNSPECIFIED., .F., .F. ) 
 B_SPLINE_CURVE_WITH_KNOTS ( ( 3, 2, 3 ),
 ( 0.4333811345117426495, 0.4500000000000000111, 0.4583811345117425051 ),
 .UNSPECIFIED. ) 
 CURVE ( )  GEOMETRIC_REPRESENTATION_ITEM ( )  RATIONAL_B_SPLINE_CURVE ( ( 0.9660722070828662300, 0.9493985675960723292, 1.000000000000000000, 0.9744809649152148534, 0.9660722070828664521 ) ) 
 REPRESENTATION_ITEM ( '' )  );
#18676 = DIRECTION ( 'NONE',  ( -0.08379744612499409606, 0.2649938410103908071, 0.9606020259449218335 ) ) ;
#18677 = VECTOR ( 'NONE', #18340, 1000.000000000000000 ) ;
#18678 = APPLICATION_PROTOCOL_DEFINITION ( 'draft international standard', 'automotive_design', 1998, #5874 ) ;
#18679 = CARTESIAN_POINT ( 'NONE',  ( -4.871646723878168217, 37.20594989384409956, 76.06675994099744287 ) ) ;
#18680 = CARTESIAN_POINT ( 'NONE',  ( 5.379229278502258182, 50.76175445474323311, 78.93590013629759028 ) ) ;
#18681 = LINE ( 'NONE', #18795, #5164 ) ;
#18682 = EDGE_LOOP ( 'NONE', ( #10123, #15595, #35, #11111, #12139, #20895 ) ) ;
#18683 = ADVANCED_FACE ( 'NONE', ( #10093 ), #16787, .F. ) ;
#18684 = CARTESIAN_POINT ( 'NONE',  ( 1.926143999677636387, 52.20300684324731577, 75.81376357423876300 ) ) ;
#18685 = AXIS2_PLACEMENT_3D ( 'NONE', #2406, #9010, #3780 ) ;
#18686 = VECTOR ( 'NONE', #8891, 1000.000000000000000 ) ;
#18687 = ORIENTED_EDGE ( 'NONE', *, *, #8807, .T. ) ;
#18688 = DIRECTION ( 'NONE',  ( -1.110223024625156540E-16, -1.000000000000000000, -5.922860397471808077E-17 ) ) ;
#18689 = CARTESIAN_POINT ( 'NONE',  ( -3.154801521863568325, 47.83913663364971569, 93.80036078214054385 ) ) ;
#18690 = CARTESIAN_POINT ( 'NONE',  ( -3.350035803220276609, 49.20851703305431357, 90.88308880123797451 ) ) ;
#18691 = B_SPLINE_SURFACE_WITH_KNOTS ( 'NONE', 3, 1, ( 
 ( #11195, #12883 ),
 ( #4991, #1722 ),
 ( #8709, #7087 ),
 ( #14478, #1826 ),
 ( #17777, #19258 ),
 ( #8201, #6590 ),
 ( #16084, #14789 ),
 ( #13098, #4673 ),
 ( #6485, #16404 ),
 ( #11512, #17984 ),
 ( #3801, #3408 ),
 ( #16794, #9918 ),
 ( #20944, #6378 ),
 ( #8311, #211 ),
 ( #19364, #3204 ),
 ( #6696, #13201 ),
 ( #17666, #12993 ),
 ( #11407, #607 ),
 ( #9706, #2210 ),
 ( #15192, #3099 ),
 ( #9602, #1507 ),
 ( #16185, #18860 ),
 ( #5564, #9194 ) ),
 .UNSPECIFIED., .F., .F., .F.,
 ( 4, 1, 1, 1, 1, 1, 1, 1, 1, 1, 1, 1, 1, 1, 1, 1, 1, 1, 1, 1, 4 ),
 ( 2, 2 ),
 ( 0.000000000000000000, 0.04338402653469398268, 0.08365674416537959013, 0.1211563976680593846, 0.1555788671761421382, 0.1872558283108043675, 0.2159034631954582228, 0.2418665822845563473, 0.2649561893498845744, 0.3085842690520175235, 0.3528342053628863995, 0.3996013663067077837, 0.4488757727682718413, 0.5007062493018590299, 0.5562201143629579292, 0.6158399466276373024, 0.6805899729784313790, 0.7509145939079137078, 0.8273700343273244773, 0.9100784481637514967, 0.9999999999999998890 ),
 ( 0.000000000000000000, 1.000000000000000000 ),
 .UNSPECIFIED. ) ;
#18692 = CARTESIAN_POINT ( 'NONE',  ( -3.384255150065147877, 52.18657681870956111, 76.19075138459079710 ) ) ;
#18693 = ORIENTED_EDGE ( 'NONE', *, *, #4599, .T. ) ;
#18694 = VECTOR ( 'NONE', #20163, 1000.000000000000000 ) ;
#18695 = AXIS2_PLACEMENT_3D ( 'NONE', #14955, #13367, #7063 ) ;
#18696 = CARTESIAN_POINT ( 'NONE',  ( -3.154801521863568325, 47.83913663364971569, 94.11286078555450274 ) ) ;
#18697 = ORIENTED_EDGE ( 'NONE', *, *, #14151, .F. ) ;
#18698 = DIRECTION ( 'NONE',  ( -0.9999689119394085113, 0.007885122365275831768, -1.526048693634352652E-16 ) ) ;
#18699 = CARTESIAN_POINT ( 'NONE',  ( -3.539401246598059991, 43.09270903039240608, 82.45433879953087342 ) ) ;
#18700 = CARTESIAN_POINT ( 'NONE',  ( -4.884656273474449861, 44.39824779480852612, 90.84496379953097289 ) ) ;
#18701 = EDGE_CURVE ( 'NONE', #264, #3603, #13616, .T. ) ;
#18702 = CARTESIAN_POINT ( 'NONE',  ( 31.03948732994507864, 36.35905713404685002, 76.90433879953100416 ) ) ;
#18703 = DIRECTION ( 'NONE',  ( 0.007885122365275663500, 0.9999689119394085113, 1.805443505845543142E-16 ) ) ;
#18704 = CARTESIAN_POINT ( 'NONE',  ( -0.9377071953849747121, 52.84024610139663025, 76.97528204790549466 ) ) ;
#18705 = DIRECTION ( 'NONE',  ( -0.9485903129789527988, 0.3165065846431829311, -8.934458285744989980E-17 ) ) ;
#18706 = LINE ( 'NONE', #14125, #7041 ) ;
#18707 = CARTESIAN_POINT ( 'NONE',  ( -5.799282478806809138, 50.46088670938467402, 76.15119298917683466 ) ) ;
#18708 =( LENGTH_UNIT ( ) NAMED_UNIT ( * ) SI_UNIT ( .MILLI., .METRE. ) );
#18709 = CARTESIAN_POINT ( 'NONE',  ( 1.256812508749381774, 49.74246873332880625, 95.17996380294498238 ) ) ;
#18710 = ADVANCED_FACE ( 'NONE', ( #13697 ), #1165, .T. ) ;
#18711 = VECTOR ( 'NONE', #4134, 1000.000000000000000 ) ;
#18712 = CARTESIAN_POINT ( 'NONE',  ( -4.537099264183358294, 37.70896829297682729, 72.45433879953085921 ) ) ;
#18713 = ORIENTED_EDGE ( 'NONE', *, *, #20758, .F. ) ;
#18714 = CARTESIAN_POINT ( 'NONE',  ( 5.678707969346596940, 37.03109401252010002, 78.30808796996917920 ) ) ;
#18715 = EDGE_CURVE ( 'NONE', #12108, #4079, #6530, .T. ) ;
#18716 = ORIENTED_EDGE ( 'NONE', *, *, #12493, .F. ) ;
#18717 = DIRECTION ( 'NONE',  ( -0.5941461771851693774, -0.8043570849667760481, -2.357623395011396791E-16 ) ) ;
#18718 = LINE ( 'NONE', #7218, #16373 ) ;
#18719 = CARTESIAN_POINT ( 'NONE',  ( -3.600277166070542378, 52.03221539514291294, 79.18928797456808866 ) ) ;
#18720 = FILL_AREA_STYLE_COLOUR ( '', #6505 ) ;
#18721 = CARTESIAN_POINT ( 'NONE',  ( -1.047061061252481107, 36.11373028406117669, 72.45433879953085921 ) ) ;
#18722 = CARTESIAN_POINT ( 'NONE',  ( -7.101199524512181505, 46.93036113559941214, 79.11815246340434271 ) ) ;
#18723 = CARTESIAN_POINT ( 'NONE',  ( 5.597054231160713655, 36.97274724074663510, 77.75916469768418438 ) ) ;
#18724 = EDGE_CURVE ( 'NONE', #15252, #5582, #11447, .T. ) ;
#18725 = CARTESIAN_POINT ( 'NONE',  ( -3.566438244846301231, 38.23101125920473464, 76.53375056423675460 ) ) ;
#18726 = ORIENTED_EDGE ( 'NONE', *, *, #5201, .F. ) ;
#18727 = ORIENTED_EDGE ( 'NONE', *, *, #6887, .F. ) ;
#18728 = UNCERTAINTY_MEASURE_WITH_UNIT (LENGTH_MEASURE( 1.000000000000000082E-05 ), #5370, 'distance_accuracy_value', 'NONE');
#18729 = CARTESIAN_POINT ( 'NONE',  ( 9.327624742576356098, 42.74920758916827168, 78.90414333341678343 ) ) ;
#18730 = CARTESIAN_POINT ( 'NONE',  ( -4.611439147851055687, 37.01374503923339176, 75.36135576041903050 ) ) ;
#18731 = CARTESIAN_POINT ( 'NONE',  ( 8.873269659708348911, 41.38747658206386149, 75.97261045075327957 ) ) ;
#18732 = CARTESIAN_POINT ( 'NONE',  ( 2.522153740306511072, 50.16218137147969713, 53.55433879953100273 ) ) ;
#18733 = CARTESIAN_POINT ( 'NONE',  ( -4.224566820778121290, 46.53527118704992915, 95.05433879953105247 ) ) ;
#18734 = CARTESIAN_POINT ( 'NONE',  ( 8.512798039827604413, 42.67153831990107449, 77.98843304575544266 ) ) ;
#18735 = CARTESIAN_POINT ( 'NONE',  ( -2.904223097202481174, 48.62752260303690122, 92.83621380294498238 ) ) ;
#18736 = AXIS2_PLACEMENT_3D ( 'NONE', #3510, #4773, #14577 ) ;
#18737 = CARTESIAN_POINT ( 'NONE',  ( -10.17784625969349399, 36.96218137147968008, 54.55433879953098852 ) ) ;
#18738 = CARTESIAN_POINT ( 'NONE',  ( -7.047711364469002149, 47.14767026684477003, 78.25347377718505015 ) ) ;
#18739 = DIRECTION ( 'NONE',  ( 0.3165065846432129626, 0.9485903129789426957, 0.000000000000000000 ) ) ;
#18740 = ADVANCED_FACE ( 'NONE', ( #13037 ), #1738, .T. ) ;
#18741 = LINE ( 'NONE', #2250, #10257 ) ;
#18742 = ORIENTED_EDGE ( 'NONE', *, *, #2645, .T. ) ;
#18743 = EDGE_CURVE ( 'NONE', #12999, #19292, #3019, .T. ) ;
#18744 = DIRECTION ( 'NONE',  ( -0.5813877811927011807, 0.8136266022444372803, 5.636455622144619183E-17 ) ) ;
#18745 = ORIENTED_EDGE ( 'NONE', *, *, #14055, .T. ) ;
#18746 = VECTOR ( 'NONE', #19589, 1000.000000000000000 ) ;
#18747 = CARTESIAN_POINT ( 'NONE',  ( -4.655845291449849377, 51.27794505956256188, 78.93463708245236887 ) ) ;
#18748 = EDGE_CURVE ( 'NONE', #8152, #11825, #14819, .T. ) ;
#18749 = AXIS2_PLACEMENT_3D ( 'NONE', #1481, #3181, #184 ) ;
#18750 = CARTESIAN_POINT ( 'NONE',  ( -2.904223097202481174, 48.62752260303690122, 95.33621380294498238 ) ) ;
#18751 = ORIENTED_EDGE ( 'NONE', *, *, #1259, .F. ) ;
#18752 = CARTESIAN_POINT ( 'NONE',  ( -1.419351766502868761, 49.49642391118513274, 94.90746379782397923 ) ) ;
#18753 = ADVANCED_FACE ( 'NONE', ( #6209, #9633 ), #40, .T. ) ;
#18754 = CARTESIAN_POINT ( 'NONE',  ( 33.61275266354798674, 51.36218137147967866, 45.55433879953098852 ) ) ;
#18755 = CARTESIAN_POINT ( 'NONE',  ( -3.218729019158923954, 51.38508014927832335, 79.24282704039583791 ) ) ;
#18756 = CARTESIAN_POINT ( 'NONE',  ( 0.8496251597415627188, 52.95608624727413627, 77.71799959699670524 ) ) ;
#18757 = CARTESIAN_POINT ( 'NONE',  ( 0.5868117437017631444, 52.36192644938283536, 77.38375056423674891 ) ) ;
#18758 = CARTESIAN_POINT ( 'NONE',  ( -4.751859364981153355, 37.11746779715601718, 79.54765774203875139 ) ) ;
#18759 = ORIENTED_EDGE ( 'NONE', *, *, #3511, .F. ) ;
#18760 = CARTESIAN_POINT ( 'NONE',  ( 6.660594192354429843, 43.89417127335556046, 93.11058879782397923 ) ) ;
#18761 = ORIENTED_EDGE ( 'NONE', *, *, #19762, .T. ) ;
#18762 = CARTESIAN_POINT ( 'NONE',  ( 3.052272305227448967, 39.76218035589567990, 95.01850678128215577 ) ) ;
#18763 = CARTESIAN_POINT ( 'NONE',  ( -3.565990957808644168, 37.05209079725128873, 75.50374684392987490 ) ) ;
#18764 = CARTESIAN_POINT ( 'NONE',  ( 6.862151516847506016, 50.41949500963030317, 77.39285358288198324 ) ) ;
#18765 = CARTESIAN_POINT ( 'NONE',  ( -7.291302197332327317, 40.11373609668280693, 78.44772760609974682 ) ) ;
#18766 = DIRECTION ( 'NONE',  ( 1.196361017915039239E-16, 0.000000000000000000, -1.000000000000000000 ) ) ;
#18767 = VECTOR ( 'NONE', #6635, 999.9999999999998863 ) ;
#18768 = CARTESIAN_POINT ( 'NONE',  ( -4.542470680087303592, 37.71301808247110188, 77.90541956767252429 ) ) ;
#18769 = CARTESIAN_POINT ( 'NONE',  ( 5.931673172199543487, 50.32702347935969556, 79.47852512212875808 ) ) ;
#18770 = AXIS2_PLACEMENT_3D ( 'NONE', #7446, #2345, #18519 ) ;
#18771 = ORIENTED_EDGE ( 'NONE', *, *, #3499, .T. ) ;
#18772 = CARTESIAN_POINT ( 'NONE',  ( 8.216412660687694824, 41.33909262012433317, 78.80099766627323277 ) ) ;
#18773 = ORIENTED_EDGE ( 'NONE', *, *, #15105, .F. ) ;
#18774 = DIRECTION ( 'NONE',  ( 1.540237394707284220E-16, 1.793354297423764243E-16, -1.000000000000000000 ) ) ;
#18775 = ADVANCED_FACE ( 'NONE', ( #11227 ), #16113, .F. ) ;
#18776 = CARTESIAN_POINT ( 'NONE',  ( -2.077846259693550746, 39.65884927180063357, 91.66433879953099506 ) ) ;
#18777 = ORIENTED_EDGE ( 'NONE', *, *, #3836, .F. ) ;
#18778 = CARTESIAN_POINT ( 'NONE',  ( 5.611423337425062385, 41.22389019960463230, 95.33621380123798872 ) ) ;
#18779 = CARTESIAN_POINT ( 'NONE',  ( -4.630794176838950449, 51.29584566888366481, 79.54703672271651271 ) ) ;
#18780 = CARTESIAN_POINT ( 'NONE',  ( 2.043125170982144745, 38.48583871533720213, 95.02371380123805977 ) ) ;
#18781 = AXIS2_PLACEMENT_3D ( 'NONE', #10613, #2707, #20665 ) ;
#18782 = CARTESIAN_POINT ( 'NONE',  ( 23.63948732994508006, 36.35905713404685002, 76.90433879953101837 ) ) ;
#18783 = CARTESIAN_POINT ( 'NONE',  ( -1.477846259693489150, 50.16218137147969713, 51.55433879953100273 ) ) ;
#18784 = VECTOR ( 'NONE', #5186, 1000.000000000000000 ) ;
#18785 = ORIENTED_EDGE ( 'NONE', *, *, #2765, .F. ) ;
#18786 = CARTESIAN_POINT ( 'NONE',  ( 29.36559987429793139, 40.36218137147969287, 87.72770477045767734 ) ) ;
#18787 = CARTESIAN_POINT ( 'NONE',  ( 0.8296073574565104858, 52.96365912811320698, 78.75172105370583608 ) ) ;
#18788 = ORIENTED_EDGE ( 'NONE', *, *, #20911, .F. ) ;
#18789 = CARTESIAN_POINT ( 'NONE',  ( -5.048451936153556474, 43.75436344969243407, 92.45433879953098710 ) ) ;
#18790 = DIRECTION ( 'NONE',  ( 0.3165065846431827645, 0.9485903129789529098, 0.000000000000000000 ) ) ;
#18791 = DIRECTION ( 'NONE',  ( 1.000000000000000000, 0.000000000000000000, 0.000000000000000000 ) ) ;
#18792 = CARTESIAN_POINT ( 'NONE',  ( 5.455409717288331350, 36.87153325707006957, 76.14053225265315916 ) ) ;
#18793 = CARTESIAN_POINT ( 'NONE',  ( 5.739147447831700610, 51.24901287804902239, 78.93590013629759028 ) ) ;
#18794 = VECTOR ( 'NONE', #18119, 1000.000000000000000 ) ;
#18795 = CARTESIAN_POINT ( 'NONE',  ( 2.643026689701002407, 51.46641972551267941, 72.45432679953087529 ) ) ;
#18796 = EDGE_CURVE ( 'NONE', #3932, #12110, #16041, .T. ) ;
#18797 = ORIENTED_EDGE ( 'NONE', *, *, #12534, .F. ) ;
#18798 = CARTESIAN_POINT ( 'NONE',  ( 0.6420704436484546695, 52.96597034637404988, 75.36071969156348871 ) ) ;
#18799 = ORIENTED_EDGE ( 'NONE', *, *, #1576, .F. ) ;
#18800 = CARTESIAN_POINT ( 'NONE',  ( 6.062166292594780792, 51.01041186941530015, 75.37891144279687694 ) ) ;
#18801 = DIRECTION ( 'NONE',  ( 0.000000000000000000, 0.000000000000000000, 1.000000000000000000 ) ) ;
#18802 = CARTESIAN_POINT ( 'NONE',  ( 3.122075258343615545, 38.59543968120053847, 90.21201841395856036 ) ) ;
#18803 = CARTESIAN_POINT ( 'NONE',  ( 0.5221537403064959726, 50.56218137147968861, 95.05433879953096721 ) ) ;
#18804 = ORIENTED_EDGE ( 'NONE', *, *, #20785, .T. ) ;
#18805 = CARTESIAN_POINT ( 'NONE',  ( -5.256821130788762453, 49.97995522249031808, 75.81950988351437104 ) ) ;
#18806 = ORIENTED_EDGE ( 'NONE', *, *, #2550, .T. ) ;
#18807 = CARTESIAN_POINT ( 'NONE',  ( 4.882729479566670250, 50.96759932735817955, 79.51138782552760631 ) ) ;
#18808 =( BOUNDED_CURVE ( )  B_SPLINE_CURVE ( 3, ( #20331, #12273, #4170, #10695 ),
 .UNSPECIFIED., .F., .F. ) 
 B_SPLINE_CURVE_WITH_KNOTS ( ( 4, 4 ),
 ( 2.801755744135677517, 3.481429563043919373 ),
 .UNSPECIFIED. ) 
 CURVE ( )  GEOMETRIC_REPRESENTATION_ITEM ( )  RATIONAL_B_SPLINE_CURVE ( ( 1.000000000000000000, 0.9618726943880423486, 0.9618726943880423486, 1.000000000000000000 ) ) 
 REPRESENTATION_ITEM ( '' )  );
#18809 = PLANE ( 'NONE',  #18337 ) ;
#18810 = CARTESIAN_POINT ( 'NONE',  ( 8.415472958870040543, 40.01543082757027747, 76.00709785348774972 ) ) ;
#18811 = VECTOR ( 'NONE', #13861, 1000.000000000000000 ) ;
#18812 = CARTESIAN_POINT ( 'NONE',  ( 5.549717964907305401, 50.64299944696890776, 75.36188203480982395 ) ) ;
#18813 = CARTESIAN_POINT ( 'NONE',  ( -6.705847964633579572, 40.30006211529013882, 78.61740305894309699 ) ) ;
#18814 = CARTESIAN_POINT ( 'NONE',  ( -7.611372734017126440, 43.12018948500615778, 78.28007409364852265 ) ) ;
#18815 = CARTESIAN_POINT ( 'NONE',  ( -4.524181921268124462, 40.28999182795290324, 94.94558880123797451 ) ) ;
#18816 = DIRECTION ( 'NONE',  ( 1.540237394707284220E-16, 1.793354297423764243E-16, -1.000000000000000000 ) ) ;
#18817 = EDGE_CURVE ( 'NONE', #10195, #1640, #18014, .T. ) ;
#18818 = CARTESIAN_POINT ( 'NONE',  ( -5.048651755005553632, 50.07748435998981762, 75.61447646545406087 ) ) ;
#18819 = CARTESIAN_POINT ( 'NONE',  ( -3.943187491250720544, 40.73580453397070755, 90.64871380294496817 ) ) ;
#18820 = CARTESIAN_POINT ( 'NONE',  ( -7.655444683876213574, 40.90690537883764222, 79.47793662387863378 ) ) ;
#18821 = FILL_AREA_STYLE_COLOUR ( '', #4764 ) ;
#18822 = ADVANCED_FACE ( 'NONE', ( #13024 ), #19499, .F. ) ;
#18823 = CIRCLE ( 'NONE', #8285, 3.200000000000009504 ) ;
#18824 = CARTESIAN_POINT ( 'NONE',  ( -7.610357185174691175, 43.11228522227810345, 75.86215519470648871 ) ) ;
#18825 = EDGE_CURVE ( 'NONE', #10514, #12777, #5516, .T. ) ;
#18826 = DIRECTION ( 'NONE',  ( -1.540237394707284220E-16, -1.793354297423764243E-16, 1.000000000000000000 ) ) ;
#18827 = CARTESIAN_POINT ( 'NONE',  ( -4.292896230825959059, 50.79981292070976906, 78.93513991157864496 ) ) ;
#18828 = CARTESIAN_POINT ( 'NONE',  ( 5.611423337425062385, 41.22389019960463230, 91.58621380123798872 ) ) ;
#18829 = PLANE ( 'NONE',  #1037 ) ;
#18830 = CARTESIAN_POINT ( 'NONE',  ( -8.093136328865547569, 42.20592732569928529, 79.45715840112796968 ) ) ;
#18831 = CARTESIAN_POINT ( 'NONE',  ( 5.442040249694054310, 36.86197992501465137, 77.64535406911728899 ) ) ;
#18832 = CARTESIAN_POINT ( 'NONE',  ( -4.421933507194019342, 37.62019378118617396, 78.93084429746392061 ) ) ;
#18833 = CARTESIAN_POINT ( 'NONE',  ( -4.677846259692849173, 45.55551717212267704, 92.65237681315549878 ) ) ;
#18834 = CARTESIAN_POINT ( 'NONE',  ( 5.427780505986065762, 36.85179043424346190, 76.70433879953087342 ) ) ;
#18835 = DIRECTION ( 'NONE',  ( -1.110223024625156540E-16, -1.000000000000000000, -5.922860397471808077E-17 ) ) ;
#18836 = LINE ( 'NONE', #12358, #5692 ) ;
#18837 = CARTESIAN_POINT ( 'NONE',  ( 8.326116433130623662, 42.11204170176992534, 78.13634973986094678 ) ) ;
#18838 = CARTESIAN_POINT ( 'NONE',  ( -4.677846259693497544, 44.16218137147969003, 77.84651775085080772 ) ) ;
#18839 = LINE ( 'NONE', #10678, #6397 ) ;
#18840 = CARTESIAN_POINT ( 'NONE',  ( 5.902048492000326441, 51.12868443877599134, 78.59183879953087626 ) ) ;
#18841 = CARTESIAN_POINT ( 'NONE',  ( 8.787829143201870252, 41.13140593384865440, 77.14698585835439815 ) ) ;
#18842 = ADVANCED_FACE ( 'NONE', ( #19598 ), #5020, .T. ) ;
#18843 = DIRECTION ( 'NONE',  ( 1.000000000000000000, 0.000000000000000000, 0.000000000000000000 ) ) ;
#18844 = ORIENTED_EDGE ( 'NONE', *, *, #12077, .F. ) ;
#18845 = CARTESIAN_POINT ( 'NONE',  ( 5.478935120625926025, 50.68658530016113417, 77.27318761637275202 ) ) ;
#18846 = ORIENTED_EDGE ( 'NONE', *, *, #16686, .T. ) ;
#18847 = CARTESIAN_POINT ( 'NONE',  ( 2.263811127080454622, 49.90383875825364157, 69.41268141275703840 ) ) ;
#18848 = CARTESIAN_POINT ( 'NONE',  ( 1.256812508749381774, 49.74246873332880625, 93.92996380294498238 ) ) ;
#18849 = ORIENTED_EDGE ( 'NONE', *, *, #12626, .T. ) ;
#18850 = CARTESIAN_POINT ( 'NONE',  ( -5.616286711741429905, 44.43019146960381960, 92.64183879782400766 ) ) ;
#18851 = CARTESIAN_POINT ( 'NONE',  ( -0.9429546156000722101, 52.21950014059650158, 77.04772206183797323 ) ) ;
#18852 = CARTESIAN_POINT ( 'NONE',  ( 9.012782495821852535, 41.80560540242532852, 78.13577067582016866 ) ) ;
#18853 = CARTESIAN_POINT ( 'NONE',  ( 6.303853310235981056, 37.47779998508790555, 78.34126521887253602 ) ) ;
#18854 = CARTESIAN_POINT ( 'NONE',  ( 0.8455663297060546091, 52.35216279802085637, 76.48963291717792856 ) ) ;
#18855 = CARTESIAN_POINT ( 'NONE',  ( 28.52215374030649997, 44.16218137147968292, 93.55433879953098142 ) ) ;
#18856 = ORIENTED_EDGE ( 'NONE', *, *, #915, .F. ) ;
#18857 = EDGE_CURVE ( 'NONE', #9111, #1841, #3437, .T. ) ;
#18858 = CARTESIAN_POINT ( 'NONE',  ( 8.319563636934814710, 41.64804018434459465, 75.98771331677210128 ) ) ;
#18859 = ORIENTED_EDGE ( 'NONE', *, *, #20923, .F. ) ;
#18860 = CARTESIAN_POINT ( 'NONE',  ( 5.287666634764763174, 37.67144577404334171, 75.36130176902827316 ) ) ;
#18861 = DIRECTION ( 'NONE',  ( 1.540237394707284220E-16, 1.793354297423764243E-16, -1.000000000000000000 ) ) ;
#18862 = EDGE_CURVE ( 'NONE', #1135, #12698, #12805, .T. ) ;
#18863 = LINE ( 'NONE', #2268, #17948 ) ;
#18864 = CARTESIAN_POINT ( 'NONE',  ( 2.891178763948851316, 49.58011693252095142, 93.16981103995755120 ) ) ;
#18865 = CARTESIAN_POINT ( 'NONE',  ( -3.350035803220276609, 49.20851703305431357, 95.72683880123798872 ) ) ;
#18866 = DIRECTION ( 'NONE',  ( 0.3165065846431829311, 0.9485903129789527988, 2.188653791613874255E-16 ) ) ;
#18867 = CARTESIAN_POINT ( 'NONE',  ( 4.666303754810079418, 40.22630141247467606, 95.62484283304920041 ) ) ;
#18868 = CARTESIAN_POINT ( 'NONE',  ( 6.484722254825411092, 49.79139610127609927, 78.65755348986731121 ) ) ;
#18869 = EDGE_CURVE ( 'NONE', #20498, #3734, #11434, .T. ) ;
#18870 = EDGE_CURVE ( 'NONE', #1841, #16818, #4701, .T. ) ;
#18871 = B_SPLINE_SURFACE_WITH_KNOTS ( 'NONE', 3, 1, ( 
 ( #17131, #11148 ),
 ( #2554, #17519 ),
 ( #2940, #9557 ),
 ( #1352, #9050 ),
 ( #15537, #7844 ),
 ( #954, #14326 ),
 ( #14216, #12634 ),
 ( #14536, #16039 ),
 ( #7946, #14429 ),
 ( #16143, #17728 ),
 ( #12832, #9661 ),
 ( #1563, #2083 ),
 ( #16662, #267 ),
 ( #6547, #14746 ),
 ( #13152, #3772 ) ),
 .UNSPECIFIED., .F., .F., .F.,
 ( 4, 1, 1, 1, 1, 1, 1, 1, 1, 1, 1, 1, 4 ),
 ( 2, 2 ),
 ( 0.000000000000000000, 0.09897586389363323411, 0.1834007553115765132, 0.2562582723958196640, 0.3272804813821422187, 0.3687296102942994591, 0.4216358900696890455, 0.4870080516106923274, 0.5645314195351998077, 0.6541098812875514312, 0.7570203673134348055, 0.8723000540617986687, 1.000000000000000000 ),
 ( 0.000000000000000000, 1.000000000000000000 ),
 .UNSPECIFIED. ) ;
#18872 = ORIENTED_EDGE ( 'NONE', *, *, #14327, .F. ) ;
#18873 = LINE ( 'NONE', #4280, #5076 ) ;
#18874 = EDGE_CURVE ( 'NONE', #4092, #11503, #8550, .T. ) ;
#18875 = VERTEX_POINT ( 'NONE', #8762 ) ;
#18876 = CARTESIAN_POINT ( 'NONE',  ( -5.590960105440975880, 48.67769231808699715, 72.45433879953087342 ) ) ;
#18877 = CARTESIAN_POINT ( 'NONE',  ( 6.828503391016846891, 43.33193468930419101, 95.41433880123797451 ) ) ;
#18878 = CARTESIAN_POINT ( 'NONE',  ( -7.080689300340610615, 41.44950609765598415, 78.61536821129558916 ) ) ;
#18879 = VERTEX_POINT ( 'NONE', #19707 ) ;
#18880 = CARTESIAN_POINT ( 'NONE',  ( -2.416137431568557314, 39.07291177436112406, 95.02371380123797451 ) ) ;
#18881 = CARTESIAN_POINT ( 'NONE',  ( -4.901409867458520253, 51.10247360423972651, 79.52300236340988704 ) ) ;
#18882 = CARTESIAN_POINT ( 'NONE',  ( -5.199045795788149071, 43.94855844323328853, 95.05433879953095300 ) ) ;
#18883 = ORIENTED_EDGE ( 'NONE', *, *, #5435, .F. ) ;
#18884 = CARTESIAN_POINT ( 'NONE',  ( 4.816229352426441679, 36.41479837022654920, 75.57109918664292536 ) ) ;
#18885 = LINE ( 'NONE', #10616, #7108 ) ;
#18886 = ORIENTED_EDGE ( 'NONE', *, *, #1451, .T. ) ;
#18887 = DIRECTION ( 'NONE',  ( 0.5813877811927011807, -0.8136266022444372803, -5.636455622144619183E-17 ) ) ;
#18888 = CARTESIAN_POINT ( 'NONE',  ( -4.524181921268124462, 40.28999182795290324, 92.44558880123798872 ) ) ;
#18889 = ORIENTED_EDGE ( 'NONE', *, *, #12093, .F. ) ;
#18890 = CARTESIAN_POINT ( 'NONE',  ( 1.456841371642047411, 39.25032235153333460, 92.45433879953097289 ) ) ;
#18891 = CARTESIAN_POINT ( 'NONE',  ( 5.278955283585622382, 37.48279278996433561, 75.97346894869129130 ) ) ;
#18892 = CARTESIAN_POINT ( 'NONE',  ( -4.812088799398940075, 42.22067586467031930, 93.96996379782397923 ) ) ;
#18893 = CARTESIAN_POINT ( 'NONE',  ( 2.522153740306494640, 49.81903562097208749, 75.21119304902340730 ) ) ;
#18894 = ADVANCED_FACE ( 'NONE', ( #5334 ), #20243, .F. ) ;
#18895 = CARTESIAN_POINT ( 'NONE',  ( 5.618638386382252214, 36.98817048782158423, 75.97391373086902888 ) ) ;
#18896 = CARTESIAN_POINT ( 'NONE',  ( -1.477846259693497366, 47.62628298661744708, 45.55433879953100273 ) ) ;
#18897 = ORIENTED_EDGE ( 'NONE', *, *, #2039, .F. ) ;
#18898 = CARTESIAN_POINT ( 'NONE',  ( 1.294600740468589306, 52.96082490517478902, 75.43490186719157009 ) ) ;
#18899 = ORIENTED_EDGE ( 'NONE', *, *, #17307, .T. ) ;
#18900 = CARTESIAN_POINT ( 'NONE',  ( 5.750640099535992533, 51.24052371918730842, 75.36022115247205022 ) ) ;
#18901 = CARTESIAN_POINT ( 'NONE',  ( 5.824017363460040286, 37.13492678543709502, 77.62670008255557264 ) ) ;
#18902 = CARTESIAN_POINT ( 'NONE',  ( -5.154188915835984375, 42.64120994080404614, 92.36746380123797451 ) ) ;
#18903 = VERTEX_POINT ( 'NONE', #8873 ) ;
#18904 = ORIENTED_EDGE ( 'NONE', *, *, #18192, .F. ) ;
#18905 = CARTESIAN_POINT ( 'NONE',  ( -3.321341072305123987, 36.98563450613462322, 75.66260743385902288 ) ) ;
#18906 = PLANE ( 'NONE',  #17770 ) ;
#18907 = ORIENTED_EDGE ( 'NONE', *, *, #6763, .F. ) ;
#18908 = DIRECTION ( 'NONE',  ( -0.8136266022444372803, -0.5813877811927012917, -2.295812393977109100E-16 ) ) ;
#18909 = CARTESIAN_POINT ( 'NONE',  ( 0.5221537403065188432, 44.16218137147969003, 54.55433879953099563 ) ) ;
#18910 = FACE_OUTER_BOUND ( 'NONE', #12159, .T. ) ;
#18911 = ORIENTED_EDGE ( 'NONE', *, *, #17449, .F. ) ;
#18912 = CARTESIAN_POINT ( 'NONE',  ( 5.916087328049406402, 50.33910869090388474, 75.42577415430537258 ) ) ;
#18913 = DIRECTION ( 'NONE',  ( 0.7071067811865479058, -3.662367542345315236E-17, -0.7071067811865472397 ) ) ;
#18914 = CARTESIAN_POINT ( 'NONE',  ( -4.454500421143473332, 37.64505674804929924, 79.54845644658969661 ) ) ;
#18915 = LINE ( 'NONE', #6413, #8071 ) ;
#18916 = CARTESIAN_POINT ( 'NONE',  ( 5.243485048422129147, 51.61513872599351771, 75.41617184184443090 ) ) ;
#18917 = CARTESIAN_POINT ( 'NONE',  ( 3.948530577815480225, 39.69684013992245752, 94.71121380294496817 ) ) ;
#18918 = LINE ( 'NONE', #18712, #3808 ) ;
#18919 = CARTESIAN_POINT ( 'NONE',  ( 8.951227662965957066, 41.62112166339042574, 78.59502675972919405 ) ) ;
#18920 = CARTESIAN_POINT ( 'NONE',  ( -0.9281697048186325905, 52.21736150593820724, 78.52473566685461037 ) ) ;
#18921 = AXIS2_PLACEMENT_3D ( 'NONE', #3747, #8667, #8444 ) ;
#18922 = CARTESIAN_POINT ( 'NONE',  ( 31.07218010054375412, 42.96218137147968008, 69.80574467885101342 ) ) ;
#18923 = CARTESIAN_POINT ( 'NONE',  ( -1.123656915330052408, 35.37488560990637865, 76.16022115247204738 ) ) ;
#18924 = CARTESIAN_POINT ( 'NONE',  ( 8.386004485381512552, 39.92711194308005673, 78.01856368782078732 ) ) ;
#18925 = LINE ( 'NONE', #6255, #13999 ) ;
#18926 = EDGE_CURVE ( 'NONE', #12946, #17868, #3318, .T. ) ;
#18927 = CARTESIAN_POINT ( 'NONE',  ( -7.235648897618376374, 46.52740783509096190, 79.45433879953087342 ) ) ;
#18928 = PLANE ( 'NONE',  #5151 ) ;
#18929 = VERTEX_POINT ( 'NONE', #20009 ) ;
#18930 = CARTESIAN_POINT ( 'NONE',  ( -4.505098289471030526, 37.68399364879952174, 78.84855896664149100 ) ) ;
#18931 = CARTESIAN_POINT ( 'NONE',  ( -3.532917577324399261, 36.21708460058427193, 78.46683879953087626 ) ) ;
#18932 = CARTESIAN_POINT ( 'NONE',  ( 8.947997572694543322, 41.61144087793389446, 76.20405737193274831 ) ) ;
#18933 = CARTESIAN_POINT ( 'NONE',  ( 0.3326973149608341562, 52.96014171822455552, 76.44919174070734869 ) ) ;
#18934 = DIRECTION ( 'NONE',  ( -0.000000000000000000, 2.168404344970984413E-15, -1.000000000000000000 ) ) ;
#18935 = PRESENTATION_LAYER_ASSIGNMENT (  '', '', ( #9444 ) ) ;
#18936 = CARTESIAN_POINT ( 'NONE',  ( -4.032707575244007359, 50.98077729755701881, 78.55785450940271630 ) ) ;
#18937 = DIRECTION ( 'NONE',  ( -1.193617070626243484E-16, -1.000000000000000000, 0.000000000000000000 ) ) ;
#18938 = CARTESIAN_POINT ( 'NONE',  ( -0.8923386585764341294, 52.84778144440528536, 78.77565085023587699 ) ) ;
#18939 = ORIENTED_EDGE ( 'NONE', *, *, #9968, .T. ) ;
#18940 = FACE_OUTER_BOUND ( 'NONE', #11349, .T. ) ;
#18941 = AXIS2_PLACEMENT_3D ( 'NONE', #20284, #16220, #20399 ) ;
#18942 = B_SPLINE_CURVE_WITH_KNOTS ( 'NONE', 3,
 ( #18498, #16696, #10328, #3909, #18279, #10435, #2218, #4014, #509, #15200 ),
 .UNSPECIFIED., .F., .F.,
 ( 4, 2, 2, 2, 4 ),
 ( 0.000000000000000000, 0.001160160651305638902, 0.002320321302611277371, 0.003480481953916916490, 0.004640642605222555610 ),
 .UNSPECIFIED. ) ;
#18943 = DIRECTION ( 'NONE',  ( -1.110223024625156540E-16, -1.000000000000000000, -5.922860397471808077E-17 ) ) ;
#18944 = VERTEX_POINT ( 'NONE', #3853 ) ;
#18945 = EDGE_CURVE ( 'NONE', #11018, #11438, #18324, .T. ) ;
#18946 = CYLINDRICAL_SURFACE ( 'NONE', #729, 5.199999999999999289 ) ;
#18947 = ORIENTED_EDGE ( 'NONE', *, *, #2997, .T. ) ;
#18948 = AXIS2_PLACEMENT_3D ( 'NONE', #16352, #170, #13536 ) ;
#18949 = CARTESIAN_POINT ( 'NONE',  ( -7.866550369700228806, 41.50330127738815378, 78.93669174070734584 ) ) ;
#18950 = CARTESIAN_POINT ( 'NONE',  ( -0.8237052942265477018, 49.18499566818285018, 91.50808880294498238 ) ) ;
#18951 = EDGE_LOOP ( 'NONE', ( #10985, #12154, #14737, #15665, #9081, #15037 ) ) ;
#18952 = CARTESIAN_POINT ( 'NONE',  ( -5.160557796315992540, 37.41935686500602287, 77.33669174070733732 ) ) ;
#18953 = DIRECTION ( 'NONE',  ( -1.540237394707284220E-16, -1.793354297423764243E-16, 1.000000000000000000 ) ) ;
#18954 = DIRECTION ( 'NONE',  ( 1.000000000000000000, 0.000000000000000000, 0.000000000000000000 ) ) ;
#18955 = FACE_OUTER_BOUND ( 'NONE', #11685, .T. ) ;
#18956 = CARTESIAN_POINT ( 'NONE',  ( 33.61275266354798674, 36.96218137147968719, 92.39963826115175038 ) ) ;
#18957 = CARTESIAN_POINT ( 'NONE',  ( -3.568428810981487231, 36.24331531840701359, 78.81697279211699936 ) ) ;
#18958 = VERTEX_POINT ( 'NONE', #2163 ) ;
#18959 = CARTESIAN_POINT ( 'NONE',  ( -3.349688636638950889, 52.21127678364309332, 76.69845644658968808 ) ) ;
#18960 = AXIS2_PLACEMENT_3D ( 'NONE', #15792, #19268, #15989 ) ;
#18961 = EDGE_CURVE ( 'NONE', #5281, #7102, #8662, .T. ) ;
#18962 = ORIENTED_EDGE ( 'NONE', *, *, #11859, .F. ) ;
#18963 = CARTESIAN_POINT ( 'NONE',  ( 4.555266191169155654, 52.12349827269967761, 77.01204236660041147 ) ) ;
#18964 = CARTESIAN_POINT ( 'NONE',  ( 5.568489401881125289, 48.03437091500646261, 95.41433880123797451 ) ) ;
#18965 = CARTESIAN_POINT ( 'NONE',  ( -4.524181921268124462, 40.28999182795290324, 96.03933880123798872 ) ) ;
#18966 = FACE_OUTER_BOUND ( 'NONE', #14723, .T. ) ;
#18967 = CARTESIAN_POINT ( 'NONE',  ( 19.23948732994504240, 43.16218137147968292, 84.70433879953101552 ) ) ;
#18968 = CARTESIAN_POINT ( 'NONE',  ( 35.92215374030650565, 51.36218137147967866, 93.55433879953098142 ) ) ;
#18969 = ORIENTED_EDGE ( 'NONE', *, *, #3505, .T. ) ;
#18970 = DIRECTION ( 'NONE',  ( -4.731737692062685363E-17, 0.7071067811865536790, 0.7071067811865414665 ) ) ;
#18971 = ADVANCED_FACE ( 'NONE', ( #10374 ), #2123, .T. ) ;
#18972 = EDGE_CURVE ( 'NONE', #14337, #4311, #11990, .T. ) ;
#18973 = ADVANCED_FACE ( 'NONE', ( #15359 ), #2579, .T. ) ;
#18974 = AXIS2_PLACEMENT_3D ( 'NONE', #3310, #9613, #6287 ) ;
#18975 = ORIENTED_EDGE ( 'NONE', *, *, #16497, .T. ) ;
#18976 = CARTESIAN_POINT ( 'NONE',  ( -3.384255150065147877, 52.18657681870956111, 76.19075138459079710 ) ) ;
#18977 = CARTESIAN_POINT ( 'NONE',  ( -5.784195910403845176, 44.99242805365518194, 96.03933880123796030 ) ) ;
#18978 = CARTESIAN_POINT ( 'NONE',  ( 5.639000274936166512, 51.32298756049275568, 75.36146177662637058 ) ) ;
#18979 = ORIENTED_EDGE ( 'NONE', *, *, #12341, .T. ) ;
#18980 = CARTESIAN_POINT ( 'NONE',  ( -4.945958930583990387, 50.15069347521357912, 79.33884456587460932 ) ) ;
#18981 = CARTESIAN_POINT ( 'NONE',  ( 0.5221537403065079630, 49.16218137147969003, 93.97886871425482980 ) ) ;
#18982 = ORIENTED_EDGE ( 'NONE', *, *, #20825, .T. ) ;
#18983 = CARTESIAN_POINT ( 'NONE',  ( 4.958128353061608706, 36.51619420082643330, 75.49492869865662215 ) ) ;
#18984 = CARTESIAN_POINT ( 'NONE',  ( -4.477846259693480491, 50.66141209518846011, 53.55433879953099563 ) ) ;
#18985 = ADVANCED_FACE ( 'NONE', ( #12276 ), #8537, .F. ) ;
#18986 = ORIENTED_EDGE ( 'NONE', *, *, #9650, .T. ) ;
#18987 = CARTESIAN_POINT ( 'NONE',  ( 11.22215374030650281, 42.96218137147968008, 73.80433879953100984 ) ) ;
#18988 = CARTESIAN_POINT ( 'NONE',  ( 6.198496396448986090, 45.68315280215533392, 91.74246380123798872 ) ) ;
#18989 = ORIENTED_EDGE ( 'NONE', *, *, #14926, .T. ) ;
#18990 = CARTESIAN_POINT ( 'NONE',  ( 0.6003407026341696096, 39.08370886253464960, 92.45433879953100131 ) ) ;
#18991 = CARTESIAN_POINT ( 'NONE',  ( 9.125273767571993488, 43.16218137147969003, 73.00433879953099847 ) ) ;
#18992 = AXIS2_PLACEMENT_3D ( 'NONE', #8308, #14888, #208 ) ;
#18993 = CARTESIAN_POINT ( 'NONE',  ( 0.2541436421823717318, 38.02374091943176637, 91.70433879782397923 ) ) ;
#18994 = CARTESIAN_POINT ( 'NONE',  ( -3.847046057864463187, 36.44911865529216755, 77.75315568452884918 ) ) ;
#18995 = CARTESIAN_POINT ( 'NONE',  ( 5.429213800673928780, 36.85281461415114279, 76.52220546472133833 ) ) ;
#18996 = CARTESIAN_POINT ( 'NONE',  ( -3.955205046931959956, 36.52901134360648427, 77.68963291717793140 ) ) ;
#18997 = VERTEX_POINT ( 'NONE', #15677 ) ;
#18998 = CARTESIAN_POINT ( 'NONE',  ( 1.087740465381641375, 52.94398708878058102, 76.77198585835439815 ) ) ;
#18999 = B_SPLINE_CURVE_WITH_KNOTS ( 'NONE', 3,
 ( #12577, #9496, #19067, #4477, #15983, #2893, #1508, #9393, #20850, #16085, #15878, #1294, #14585, #3410, #113, #3517, #12, #9707, #13202 ),
 .UNSPECIFIED., .F., .F.,
 ( 4, 1, 1, 1, 1, 1, 1, 1, 1, 1, 1, 1, 1, 1, 1, 1, 4 ),
 ( 0.000000000000000000, 0.09548257688036490554, 0.1831260162920692325, 0.2638843215906733763, 0.3377405854367836469, 0.4051287172156797234, 0.4664893278449969150, 0.5228337310946251648, 0.5750047063118850499, 0.6251976803793458659, 0.6747285784134858799, 0.7246222549260739054, 0.7756163566473811555, 0.8279184090424840381, 0.8823814665238148836, 0.9394578349448057253, 1.000000000000000000 ),
 .UNSPECIFIED. ) ;
#19000 = EDGE_LOOP ( 'NONE', ( #19944, #16218, #9001, #19898 ) ) ;
#19001 = CARTESIAN_POINT ( 'NONE',  ( 6.817737414320570899, 50.45230191805777054, 75.81347835631012799 ) ) ;
#19002 = EDGE_CURVE ( 'NONE', #15934, #10780, #14012, .T. ) ;
#19003 = CARTESIAN_POINT ( 'NONE',  ( 5.278470088661848969, 37.49201410884710128, 77.76022115247205591 ) ) ;
#19004 = CARTESIAN_POINT ( 'NONE',  ( 4.394343283833276992, 39.11584570990505938, 92.75808880123797451 ) ) ;
#19005 = CARTESIAN_POINT ( 'NONE',  ( 8.162892682119435861, 41.62284976526770208, 79.54845644658969661 ) ) ;
#19006 = VERTEX_POINT ( 'NONE', #10794 ) ;
#19007 = CIRCLE ( 'NONE', #15964, 3.999999999999996447 ) ;
#19008 = ORIENTED_EDGE ( 'NONE', *, *, #4760, .T. ) ;
#19009 = CARTESIAN_POINT ( 'NONE',  ( -7.948598133434920499, 41.77757099202272428, 78.60633299199227508 ) ) ;
#19010 = EDGE_CURVE ( 'NONE', #16704, #15408, #2482, .T. ) ;
#19011 = CARTESIAN_POINT ( 'NONE',  ( 6.635267586053948285, 39.64667042487232607, 72.45433879953087342 ) ) ;
#19012 = ORIENTED_EDGE ( 'NONE', *, *, #3277, .F. ) ;
#19013 = CARTESIAN_POINT ( 'NONE',  ( 4.989364768915854675, 51.80284713987553857, 79.39429067157672648 ) ) ;
#19014 = CARTESIAN_POINT ( 'NONE',  ( -6.710423945119504019, 40.29826376337096150, 78.59662358701670826 ) ) ;
#19015 = CARTESIAN_POINT ( 'NONE',  ( -3.134114116279071549, 48.15229756555780227, 90.68871379953098710 ) ) ;
#19016 = ADVANCED_FACE ( 'NONE', ( #877 ), #7362, .T. ) ;
#19017 = AXIS2_PLACEMENT_3D ( 'NONE', #10278, #3452, #251 ) ;
#19018 = VERTEX_POINT ( 'NONE', #14069 ) ;
#19019 = CARTESIAN_POINT ( 'NONE',  ( -7.687459971419651872, 40.91832003046048527, 79.47750830342025097 ) ) ;
#19020 = CARTESIAN_POINT ( 'NONE',  ( 27.03948732994508219, 27.61837231449496599, 78.60433879953100700 ) ) ;
#19021 = CARTESIAN_POINT ( 'NONE',  ( -0.9988176903691428077, 49.83852402762217082, 93.30496380123798872 ) ) ;
#19022 = CARTESIAN_POINT ( 'NONE',  ( 31.03948732994507864, 36.35905713404685002, 77.50433879953099847 ) ) ;
#19023 = VECTOR ( 'NONE', #4712, 1000.000000000000000 ) ;
#19024 = CARTESIAN_POINT ( 'NONE',  ( 5.639000274936166512, 51.32298756049275568, 75.36146177662637058 ) ) ;
#19025 = CARTESIAN_POINT ( 'NONE',  ( 7.860711257786343609, 47.82081138319720282, 79.44551527011911674 ) ) ;
#19026 = AXIS2_PLACEMENT_3D ( 'NONE', #587, #5687, #2515 ) ;
#19027 = AXIS2_PLACEMENT_3D ( 'NONE', #14738, #11764, #5463 ) ;
#19028 = CARTESIAN_POINT ( 'NONE',  ( 0.5221537403065015237, 49.16218137147969003, 92.72886871425484401 ) ) ;
#19029 = B_SPLINE_CURVE_WITH_KNOTS ( 'NONE', 3,
 ( #506, #8393, #18276, #10214, #18178, #11495, #3805, #6983 ),
 .UNSPECIFIED., .F., .F.,
 ( 4, 2, 2, 4 ),
 ( 0.000000000000000000, 0.0002641548125319239651, 0.0003962322187978856223, 0.0005283096250638472796 ),
 .UNSPECIFIED. ) ;
#19030 = CARTESIAN_POINT ( 'NONE',  ( 8.375262368375963717, 41.81499272476909113, 78.48252796260671005 ) ) ;
#19031 = CARTESIAN_POINT ( 'NONE',  ( -0.9406373985668743387, 52.21745981828536998, 78.20877650441246942 ) ) ;
#19032 = VECTOR ( 'NONE', #5157, 1000.000000000000000 ) ;
#19033 = EDGE_LOOP ( 'NONE', ( #1448, #7809, #3122, #3799 ) ) ;
#19034 = CARTESIAN_POINT ( 'NONE',  ( -4.677846259693498432, 44.16218137147969003, 92.70661078214052964 ) ) ;
#19035 = VECTOR ( 'NONE', #10753, 1000.000000000000114 ) ;
#19036 = FACE_OUTER_BOUND ( 'NONE', #14820, .T. ) ;
#19037 = CARTESIAN_POINT ( 'NONE',  ( 5.740585635973905809, 51.24795054640212300, 75.97198585835440099 ) ) ;
#19038 = SURFACE_STYLE_FILL_AREA ( #15954 ) ;
#19039 = EDGE_LOOP ( 'NONE', ( #715, #10719, #1777, #16003 ) ) ;
#19040 = CARTESIAN_POINT ( 'NONE',  ( 5.544968037009670780, 45.50804040601273925, 94.63308879953099506 ) ) ;
#19041 = CARTESIAN_POINT ( 'NONE',  ( 5.376021338371314684, 37.56172066031027867, 75.98270377909689444 ) ) ;
#19042 = EDGE_CURVE ( 'NONE', #1372, #12487, #4371, .T. ) ;
#19043 = AXIS2_PLACEMENT_3D ( 'NONE', #5394, #3910, #14993 ) ;
#19044 = ORIENTED_EDGE ( 'NONE', *, *, #10411, .F. ) ;
#19045 = VECTOR ( 'NONE', #16104, 1000.000000000000000 ) ;
#19046 = CARTESIAN_POINT ( 'NONE',  ( -1.348357406114872203, 47.70104341108812918, 69.28382765310961133 ) ) ;
#19047 = CARTESIAN_POINT ( 'NONE',  ( -3.635499589166287127, 36.29285780047638355, 79.01720576857120193 ) ) ;
#19048 = LINE ( 'NONE', #1593, #11610 ) ;
#19049 = DIRECTION ( 'NONE',  ( 1.000000000000000000, 0.000000000000000000, 0.000000000000000000 ) ) ;
#19050 = B_SPLINE_SURFACE_WITH_KNOTS ( 'NONE', 3, 1, ( 
 ( #18294, #5630 ),
 ( #18513, #18405 ),
 ( #20092, #10234 ),
 ( #12137, #13725 ),
 ( #16711, #849 ),
 ( #5305, #2135 ),
 ( #15331, #20198 ),
 ( #3825, #13506 ),
 ( #11722, #16817 ),
 ( #8731, #18615 ),
 ( #4030, #524 ) ),
 .UNSPECIFIED., .F., .F., .F.,
 ( 4, 1, 1, 1, 1, 1, 1, 1, 4 ),
 ( 2, 2 ),
 ( 0.000000000000000000, 0.1975140844462248968, 0.3638949407180063211, 0.4989527813026914393, 0.6061909113956662765, 0.6984313814761610173, 0.7906255499708312318, 0.8898677993983585832, 1.000000000000000000 ),
 ( 0.000000000000000000, 1.000000000000000000 ),
 .UNSPECIFIED. ) ;
#19051 = CARTESIAN_POINT ( 'NONE',  ( 3.178197289651381485, 47.10421403348819780, 98.25514354869233102 ) ) ;
#19052 = VECTOR ( 'NONE', #14948, 1000.000000000000000 ) ;
#19053 = DIRECTION ( 'NONE',  ( -1.301042606982606060E-16, -1.000000000000000000, 0.000000000000000000 ) ) ;
#19054 = CARTESIAN_POINT ( 'NONE',  ( 0.5221537403065020788, 52.36218137147968577, 52.53721119516358584 ) ) ;
#19055 = ORIENTED_EDGE ( 'NONE', *, *, #6503, .T. ) ;
#19056 = CARTESIAN_POINT ( 'NONE',  ( 2.043125170982144745, 38.48583871533720213, 91.27371380123798872 ) ) ;
#19057 =( GEOMETRIC_REPRESENTATION_CONTEXT ( 3 ) GLOBAL_UNCERTAINTY_ASSIGNED_CONTEXT ( ( #1679 ) ) GLOBAL_UNIT_ASSIGNED_CONTEXT ( ( #18708, #2540, #4640 ) ) REPRESENTATION_CONTEXT ( 'NONE', 'WORKASPACE' ) );
#19058 = EDGE_CURVE ( 'NONE', #18554, #3669, #1200, .T. ) ;
#19059 = CARTESIAN_POINT ( 'NONE',  ( 0.6956764376626823898, 52.36037053019133225, 78.90962006023684694 ) ) ;
#19060 = CARTESIAN_POINT ( 'NONE',  ( 5.389492195292208798, 36.82443100924615464, 78.09625056423675460 ) ) ;
#19061 = ORIENTED_EDGE ( 'NONE', *, *, #17628, .T. ) ;
#19062 = CARTESIAN_POINT ( 'NONE',  ( 8.722153740306517022, 44.16218137147969003, 54.55433879953099563 ) ) ;
#19063 = CARTESIAN_POINT ( 'NONE',  ( -3.943187491250720544, 40.73580453397070755, 94.39871380294496817 ) ) ;
#19064 = ORIENTED_EDGE ( 'NONE', *, *, #11523, .T. ) ;
#19065 = FACE_OUTER_BOUND ( 'NONE', #16982, .T. ) ;
#19066 = CARTESIAN_POINT ( 'NONE',  ( 31.07218010054375412, 42.76218137147968434, 69.80574467885101342 ) ) ;
#19067 = CARTESIAN_POINT ( 'NONE',  ( 5.603594163910166515, 51.34914062846251426, 79.54621928524807117 ) ) ;
#19068 = CARTESIAN_POINT ( 'NONE',  ( 8.832380548758539618, 43.45507459029314390, 95.45352954694192249 ) ) ;
#19069 = CARTESIAN_POINT ( 'NONE',  ( 0.5940733232197880076, 52.96558880458736240, 75.97241503363285631 ) ) ;
#19070 = CARTESIAN_POINT ( 'NONE',  ( -4.036259049554215217, 37.50289767551729625, 79.53329352641277694 ) ) ;
#19071 = ORIENTED_EDGE ( 'NONE', *, *, #5001, .F. ) ;
#19072 = CARTESIAN_POINT ( 'NONE',  ( -5.462576778579502523, 43.73439565840071452, 82.45433879953087342 ) ) ;
#19073 = CARTESIAN_POINT ( 'NONE',  ( 5.801534520520057470, 37.11886136902160160, 77.67950998295866327 ) ) ;
#19074 = ORIENTED_EDGE ( 'NONE', *, *, #8590, .F. ) ;
#19075 = CARTESIAN_POINT ( 'NONE',  ( 35.92215374030650565, 51.36218137147967866, 93.55433879953098142 ) ) ;
#19076 = ADVANCED_FACE ( 'NONE', ( #16295 ), #4676, .F. ) ;
#19077 = CARTESIAN_POINT ( 'NONE',  ( -4.524181921268124462, 40.28999182795290324, 94.78933880123798872 ) ) ;
#19078 = DIRECTION ( 'NONE',  ( -1.540237394707284220E-16, -1.793354297423764243E-16, 1.000000000000000000 ) ) ;
#19079 = CARTESIAN_POINT ( 'NONE',  ( -4.650819492866522964, 37.79909575829982060, 77.90150431758111438 ) ) ;
#19080 = CARTESIAN_POINT ( 'NONE',  ( -7.339959452894645686, 41.85620932255213233, 78.89026057757155286 ) ) ;
#19081 = VECTOR ( 'NONE', #18744, 1000.000000000000227 ) ;
#19082 = VERTEX_POINT ( 'NONE', #3304 ) ;
#19083 = CARTESIAN_POINT ( 'NONE',  ( 8.217904656458664192, 41.33102757626289758, 76.21346532620796665 ) ) ;
#19084 = VECTOR ( 'NONE', #1840, 1000.000000000000000 ) ;
#19085 = VERTEX_POINT ( 'NONE', #12686 ) ;
#19086 = CARTESIAN_POINT ( 'NONE',  ( -3.623336461783060791, 52.01573806668144329, 75.70044805065693083 ) ) ;
#19087 = EDGE_CURVE ( 'NONE', #347, #19613, #1511, .T. ) ;
#19088 = CARTESIAN_POINT ( 'NONE',  ( -4.500660556396669065, 42.81632233694663370, 91.50808879953098085 ) ) ;
#19089 = CARTESIAN_POINT ( 'NONE',  ( -7.803183483682971655, 41.28366174159560842, 78.36017682096837689 ) ) ;
#19090 = EDGE_LOOP ( 'NONE', ( #6750, #8587, #11851, #19529 ) ) ;
#19091 = CARTESIAN_POINT ( 'NONE',  ( 5.052198367669452850, 48.31320248322254685, 94.51683879782399345 ) ) ;
#19092 = CARTESIAN_POINT ( 'NONE',  ( 4.394792124162911762, 36.11365475671116343, 76.60595702694484999 ) ) ;
#19093 = CARTESIAN_POINT ( 'NONE',  ( 5.653389158101303380, 51.31235907211823388, 75.98863418974025308 ) ) ;
#19094 = EDGE_LOOP ( 'NONE', ( #779, #20738, #15154, #10157 ) ) ;
#19095 = CARTESIAN_POINT ( 'NONE',  ( -0.2125050281363792815, 38.58189400963056670, 92.99246379953098085 ) ) ;
#19096 = CARTESIAN_POINT ( 'NONE',  ( 0.8388742597782140598, 52.96358605518274487, 78.70464370717459701 ) ) ;
#19097 = AXIS2_PLACEMENT_3D ( 'NONE', #16137, #7628, #20591 ) ;
#19098 = EDGE_LOOP ( 'NONE', ( #12326, #17896, #17639, #7839 ) ) ;
#19099 = CARTESIAN_POINT ( 'NONE',  ( -4.721961219230297324, 42.48895494285373786, 92.45433879953101552 ) ) ;
#19100 = CARTESIAN_POINT ( 'NONE',  ( 6.014045509560256519, 43.93915269363458265, 95.05433879953099563 ) ) ;
#19101 = VECTOR ( 'NONE', #14529, 1000.000000000000000 ) ;
#19102 = CARTESIAN_POINT ( 'NONE',  ( 2.463659247115866258, 38.82793883177424732, 94.28246379782397923 ) ) ;
#19103 = CARTESIAN_POINT ( 'NONE',  ( 5.644533139590786064, 37.00667393039697828, 75.97264893529829521 ) ) ;
#19104 = CARTESIAN_POINT ( 'NONE',  ( 5.605329808110463219, 51.34785857800776654, 78.76051003739772227 ) ) ;
#19105 = DIRECTION ( 'NONE',  ( -1.000000000000000000, 0.000000000000000000, 0.000000000000000000 ) ) ;
#19106 = ORIENTED_EDGE ( 'NONE', *, *, #19375, .F. ) ;
#19107 = CARTESIAN_POINT ( 'NONE',  ( -7.154050613567645378, 47.04591530683940448, 77.81003234944267888 ) ) ;
#19108 = VERTEX_POINT ( 'NONE', #7786 ) ;
#19109 = VECTOR ( 'NONE', #15746, 1000.000000000000000 ) ;
#19110 = CARTESIAN_POINT ( 'NONE',  ( 33.61275266354798674, 51.36218137147967866, 93.55433879953098142 ) ) ;
#19111 = FACE_OUTER_BOUND ( 'NONE', #20943, .T. ) ;
#19112 = CARTESIAN_POINT ( 'NONE',  ( -0.9988176903691428077, 49.83852402762217082, 95.64871380123798872 ) ) ;
#19113 = VECTOR ( 'NONE', #9692, 1000.000000000000000 ) ;
#19114 = CARTESIAN_POINT ( 'NONE',  ( 8.140610423635045834, 41.55606842302987047, 79.54734031390459847 ) ) ;
#19115 = ORIENTED_EDGE ( 'NONE', *, *, #10386, .F. ) ;
#19116 = ORIENTED_EDGE ( 'NONE', *, *, #19255, .F. ) ;
#19117 = CARTESIAN_POINT ( 'NONE',  ( 11.22215374030650281, 42.76218137147968434, 62.80715055817104542 ) ) ;
#19118 = DIRECTION ( 'NONE',  ( -0.8136266022444382795, -0.5813877811926999595, -2.295812393977108607E-16 ) ) ;
#19119 = CARTESIAN_POINT ( 'NONE',  ( -5.044784019589553026, 50.18482011045266944, 75.55565227853020360 ) ) ;
#19120 = EDGE_LOOP ( 'NONE', ( #2683, #11074, #10898, #10132 ) ) ;
#19121 = CARTESIAN_POINT ( 'NONE',  ( 5.603594163910166515, 51.34914062846251426, 79.54621928524807117 ) ) ;
#19122 = CARTESIAN_POINT ( 'NONE',  ( 8.850663652843866913, 41.31972494539268581, 77.52203278780699236 ) ) ;
#19123 = CARTESIAN_POINT ( 'NONE',  ( 8.475713225669114337, 40.19597472873837063, 75.74322883085581282 ) ) ;
#19124 = ORIENTED_EDGE ( 'NONE', *, *, #15039, .F. ) ;
#19125 = CARTESIAN_POINT ( 'NONE',  ( -5.130197398460194513, 37.39693086210137807, 77.90166954077812989 ) ) ;
#19126 = CARTESIAN_POINT ( 'NONE',  ( -7.449024937915255329, 40.16431357463694241, 78.92129748799239053 ) ) ;
#19127 = CARTESIAN_POINT ( 'NONE',  ( 6.127653894365867160, 38.17679652135131363, 75.57100681021411503 ) ) ;
#19128 = CARTESIAN_POINT ( 'NONE',  ( -4.524181921268124462, 40.28999182795290324, 96.03933880123798872 ) ) ;
#19129 = EDGE_CURVE ( 'NONE', #19214, #4579, #12990, .T. ) ;
#19130 = CIRCLE ( 'NONE', #4175, 4.200000000000003730 ) ;
#19131 = CIRCLE ( 'NONE', #11949, 8.199999999999995737 ) ;
#19132 = EDGE_CURVE ( 'NONE', #19783, #20542, #16189, .T. ) ;
#19133 = CARTESIAN_POINT ( 'NONE',  ( 6.448515921954562913, 38.49488593426744387, 77.41134261343162848 ) ) ;
#19134 = DIRECTION ( 'NONE',  ( -2.775557561562892929E-15, -1.000000000000000000, 0.000000000000000000 ) ) ;
#19135 = EDGE_CURVE ( 'NONE', #14974, #9657, #14482, .T. ) ;
#19136 = DIRECTION ( 'NONE',  ( 0.4472135954999563734, 0.7745966692414840704, 0.4472135954999582608 ) ) ;
#19137 = LINE ( 'NONE', #7651, #8475 ) ;
#19138 = VERTEX_POINT ( 'NONE', #19473 ) ;
#19139 = DIRECTION ( 'NONE',  ( 1.540237394707284220E-16, 1.793354297423764243E-16, -1.000000000000000000 ) ) ;
#19140 = CARTESIAN_POINT ( 'NONE',  ( 9.353817388681445522, 42.82770861117572281, 77.06316232894263862 ) ) ;
#19141 = CARTESIAN_POINT ( 'NONE',  ( 5.561379608955574483, 51.38032281970146897, 76.39036821129558064 ) ) ;
#19142 = CARTESIAN_POINT ( 'NONE',  ( 1.352400422481993658, 50.46853102219002096, 90.72683880123797451 ) ) ;
#19143 = EDGE_CURVE ( 'NONE', #13434, #3547, #1400, .T. ) ;
#19144 = ORIENTED_EDGE ( 'NONE', *, *, #5321, .T. ) ;
#19145 = CIRCLE ( 'NONE', #5886, 3.999999999999996447 ) ;
#19146 = CARTESIAN_POINT ( 'NONE',  ( -4.537099264183359182, 37.70896829297682729, 78.53742703482498655 ) ) ;
#19147 = DIRECTION ( 'NONE',  ( -1.402518428993831183E-16, 1.000000000000000000, -3.469446951953617640E-16 ) ) ;
#19148 = DIRECTION ( 'NONE',  ( 1.000000000000000000, 0.000000000000000000, 0.000000000000000000 ) ) ;
#19149 = CARTESIAN_POINT ( 'NONE',  ( 5.647726803872021861, 51.31654162509386907, 77.98642840401727483 ) ) ;
#19150 = CARTESIAN_POINT ( 'NONE',  ( 6.519924314245371555, 49.74745151145329203, 76.63889762306028786 ) ) ;
#19151 = CARTESIAN_POINT ( 'NONE',  ( 30.92220646078100188, 45.56218137147968861, 56.80715055817104542 ) ) ;
#19152 = CARTESIAN_POINT ( 'NONE',  ( 6.946924939155297629, 50.35687629745329019, 76.28194508213313441 ) ) ;
#19153 = VECTOR ( 'NONE', #12767, 1000.000000000000114 ) ;
#19154 = EDGE_CURVE ( 'NONE', #16593, #17446, #17988, .T. ) ;
#19155 = CARTESIAN_POINT ( 'NONE',  ( -5.747619332630494959, 37.85299557360038136, 79.28390783734228364 ) ) ;
#19156 = CARTESIAN_POINT ( 'NONE',  ( -5.484081776600456593, 50.68611759094706315, 79.26884812577799266 ) ) ;
#19157 = CARTESIAN_POINT ( 'NONE',  ( 5.290600780953200299, 50.83315677396375776, 78.89498996766396033 ) ) ;
#19158 = LINE ( 'NONE', #19062, #7137 ) ;
#19159 = CARTESIAN_POINT ( 'NONE',  ( 4.987494971863720927, 47.58855820898865829, 91.27371380294496817 ) ) ;
#19160 = VERTEX_POINT ( 'NONE', #15881 ) ;
#19161 = LINE ( 'NONE', #288, #15755 ) ;
#19162 = CARTESIAN_POINT ( 'NONE',  ( -0.8928399825707434845, 52.97829838868407393, 76.13122899883298089 ) ) ;
#19163 = LINE ( 'NONE', #2679, #2348 ) ;
#19164 = DIRECTION ( 'NONE',  ( 1.000000000000000000, -0.000000000000000000, -0.000000000000000000 ) ) ;
#19165 = CARTESIAN_POINT ( 'NONE',  ( 26.27839330960315678, 64.06566441348024910, 85.06527890720687424 ) ) ;
#19166 = ORIENTED_EDGE ( 'NONE', *, *, #1576, .T. ) ;
#19167 = CARTESIAN_POINT ( 'NONE',  ( 8.882424425600639495, 41.41491399621057923, 75.97389479739716478 ) ) ;
#19168 = EDGE_LOOP ( 'NONE', ( #4798, #7635, #12756, #3423 ) ) ;
#19169 = LINE ( 'NONE', #12482, #14546 ) ;
#19170 = CARTESIAN_POINT ( 'NONE',  ( -5.154188915835984375, 42.64120994080404614, 95.96121380123798872 ) ) ;
#19171 = CARTESIAN_POINT ( 'NONE',  ( 0.4001462726638131961, 52.36130254314756627, 76.02501926799072862 ) ) ;
#19172 = CARTESIAN_POINT ( 'NONE',  ( 5.840776426723270021, 37.14690219845653019, 76.14207271482608519 ) ) ;
#19173 = LINE ( 'NONE', #6084, #5512 ) ;
#19174 = ORIENTED_EDGE ( 'NONE', *, *, #20892, .F. ) ;
#19175 = CARTESIAN_POINT ( 'NONE',  ( 8.299662904660788598, 41.56403757284476796, 75.97198585835440099 ) ) ;
#19176 = ORIENTED_EDGE ( 'NONE', *, *, #6345, .F. ) ;
#19177 = CARTESIAN_POINT ( 'NONE',  ( -3.396200966244447450, 52.17804077583208766, 76.13050287850805375 ) ) ;
#19178 = CARTESIAN_POINT ( 'NONE',  ( 1.352400422481993658, 50.46853102219002096, 93.22683880123798872 ) ) ;
#19179 = CARTESIAN_POINT ( 'NONE',  ( 4.611425380024144260, 52.08201574212262130, 75.94315254166910734 ) ) ;
#19180 = ORIENTED_EDGE ( 'NONE', *, *, #12314, .T. ) ;
#19181 = EDGE_CURVE ( 'NONE', #11953, #14920, #17251, .T. ) ;
#19182 = CARTESIAN_POINT ( 'NONE',  ( -5.819820656548302829, 50.44621087952127425, 78.57924047249254329 ) ) ;
#19183 = PLANE ( 'NONE',  #11316 ) ;
#19184 = ORIENTED_EDGE ( 'NONE', *, *, #3008, .T. ) ;
#19185 = CARTESIAN_POINT ( 'NONE',  ( 6.870794506624137377, 37.88291540698485704, 77.55645576794258034 ) ) ;
#19186 = CARTESIAN_POINT ( 'NONE',  ( -4.052506615097486886, 50.96215335582491690, 78.79092181577959764 ) ) ;
#19187 = DIRECTION ( 'NONE',  ( -5.626130192357176673E-16, -1.831515347669941892E-30, 1.000000000000000000 ) ) ;
#19188 = ORIENTED_EDGE ( 'NONE', *, *, #7748, .T. ) ;
#19189 = DIRECTION ( 'NONE',  ( -0.5813877811927011807, 0.8136266022444372803, 5.636455622144619183E-17 ) ) ;
#19190 = CARTESIAN_POINT ( 'NONE',  ( 2.043125170982144745, 38.48583871533720213, 91.42996380123798872 ) ) ;
#19191 = VERTEX_POINT ( 'NONE', #19264 ) ;
#19192 = CARTESIAN_POINT ( 'NONE',  ( 4.453501277845357542, 51.28465290960308920, 77.76130678786321937 ) ) ;
#19193 = FACE_OUTER_BOUND ( 'NONE', #17673, .T. ) ;
#19194 = DIRECTION ( 'NONE',  ( 3.211742425186504723E-16, -5.922860397471811774E-17, 1.000000000000000000 ) ) ;
#19195 = CARTESIAN_POINT ( 'NONE',  ( -4.007890887056451135, 40.01116025973682611, 92.79808879782397923 ) ) ;
#19196 = CARTESIAN_POINT ( 'NONE',  ( 8.789147962602239517, 47.20595287382010241, 75.43669174070734584 ) ) ;
#19197 = LINE ( 'NONE', #4612, #5080 ) ;
#19198 = CARTESIAN_POINT ( 'NONE',  ( -3.579922675594004122, 36.25180537319517526, 77.38751485876633751 ) ) ;
#19199 = ORIENTED_EDGE ( 'NONE', *, *, #4327, .T. ) ;
#19200 = CARTESIAN_POINT ( 'NONE',  ( 2.115822401559540378, 52.95418708249595596, 78.45122513788126639 ) ) ;
#19201 = CARTESIAN_POINT ( 'NONE',  ( -3.899559394394521483, 36.48790814162069296, 77.72081520951157074 ) ) ;
#19202 = EDGE_LOOP ( 'NONE', ( #7942, #12612, #18799, #5432, #6015 ) ) ;
#19203 = CARTESIAN_POINT ( 'NONE',  ( 1.853156886157175220, 39.32573803590444328, 92.47037068331223963 ) ) ;
#19204 = CARTESIAN_POINT ( 'NONE',  ( 11.22215374030650281, 42.76218137147968434, 74.20433879953100131 ) ) ;
#19205 = CARTESIAN_POINT ( 'NONE',  ( 8.530649028577993676, 48.02340768410154936, 78.56977997600147035 ) ) ;
#19206 = CARTESIAN_POINT ( 'NONE',  ( -2.955076890380592847, 51.58841534450542099, 76.19553520931087576 ) ) ;
#19207 = ORIENTED_EDGE ( 'NONE', *, *, #20265, .T. ) ;
#19208 = DIRECTION ( 'NONE',  ( 1.000000000000000000, 0.000000000000000000, -0.000000000000000000 ) ) ;
#19209 = EDGE_LOOP ( 'NONE', ( #1741, #18889, #3307, #12400 ) ) ;
#19210 = EDGE_CURVE ( 'NONE', #3254, #11401, #1615, .T. ) ;
#19211 = CARTESIAN_POINT ( 'NONE',  ( -3.492483110108918876, 37.11205023543848114, 75.53057231289058393 ) ) ;
#19212 = DIRECTION ( 'NONE',  ( 1.540237394707283727E-16, 1.793354297423763257E-16, -1.000000000000000000 ) ) ;
#19213 = CARTESIAN_POINT ( 'NONE',  ( 31.22215374030650281, 42.76218137147968434, 77.80433879953099563 ) ) ;
#19214 = VERTEX_POINT ( 'NONE', #9710 ) ;
#19215 = CARTESIAN_POINT ( 'NONE',  ( -4.175129846843772974, 37.46622205296527142, 77.09144163344554102 ) ) ;
#19216 = DIRECTION ( 'NONE',  ( -0.7071067811865434649, -0.7071067811865515695, 0.000000000000000000 ) ) ;
#19217 = CARTESIAN_POINT ( 'NONE',  ( 0.7582201636353277374, 49.56899138526064519, 94.28246379953097289 ) ) ;
#19218 = ORIENTED_EDGE ( 'NONE', *, *, #15769, .T. ) ;
#19219 = CARTESIAN_POINT ( 'NONE',  ( -7.775370309202131125, 41.23112419541227069, 78.65672026662821281 ) ) ;
#19220 = CARTESIAN_POINT ( 'NONE',  ( -7.872343237160707830, 41.50297897882735043, 79.54775079867083321 ) ) ;
#19221 = CARTESIAN_POINT ( 'NONE',  ( 5.475233562466685022, 37.62638353493751708, 75.36365925760465245 ) ) ;
#19222 = CARTESIAN_POINT ( 'NONE',  ( -5.154188915835984375, 42.64120994080404614, 95.96121380123798872 ) ) ;
#19223 = EDGE_CURVE ( 'NONE', #20830, #11304, #10980, .T. ) ;
#19224 = CARTESIAN_POINT ( 'NONE',  ( 3.122153740306552905, 48.66551347115873227, 90.10183880294498238 ) ) ;
#19225 = ADVANCED_FACE ( 'NONE', ( #11411 ), #8206, .T. ) ;
#19226 = CARTESIAN_POINT ( 'NONE',  ( 0.8503282811412335995, 52.95606000782370870, 76.48963291717792856 ) ) ;
#19227 = CARTESIAN_POINT ( 'NONE',  ( 13.32022995165973001, 51.36218137147968577, 92.39963826115175038 ) ) ;
#19228 = CARTESIAN_POINT ( 'NONE',  ( -0.8886661993129779669, 52.97949073723408731, 78.78847851419276083 ) ) ;
#19229 = ORIENTED_EDGE ( 'NONE', *, *, #14698, .F. ) ;
#19230 = CARTESIAN_POINT ( 'NONE',  ( 0.5221537403065005245, 44.16218137147968292, 82.45433879953087342 ) ) ;
#19231 = LINE ( 'NONE', #10759, #14329 ) ;
#19232 = EDGE_CURVE ( 'NONE', #17731, #10499, #13621, .T. ) ;
#19233 = CARTESIAN_POINT ( 'NONE',  ( 5.581171587375775900, 51.36570328251199413, 76.09992453055346573 ) ) ;
#19234 = CARTESIAN_POINT ( 'NONE',  ( 6.341737852742077131, 49.88988861453574941, 77.88538524077617353 ) ) ;
#19235 = ADVANCED_FACE ( 'NONE', ( #9924 ), #13419, .F. ) ;
#19236 = EDGE_CURVE ( 'NONE', #13342, #12496, #2028, .T. ) ;
#19237 = VERTEX_POINT ( 'NONE', #11726 ) ;
#19238 = EDGE_CURVE ( 'NONE', #4532, #13937, #11692, .T. ) ;
#19239 = VERTEX_POINT ( 'NONE', #317 ) ;
#19240 = CARTESIAN_POINT ( 'NONE',  ( 8.530649028577993676, 48.02340768410154936, 78.56977997600147035 ) ) ;
#19241 = CARTESIAN_POINT ( 'NONE',  ( -4.032470478286651172, 50.98093479776591863, 76.41531757229334687 ) ) ;
#19242 = EDGE_CURVE ( 'NONE', #7731, #13604, #15012, .T. ) ;
#19243 = CARTESIAN_POINT ( 'NONE',  ( 5.250115436669491764, 37.46233028808841681, 77.75922307965579705 ) ) ;
#19244 = CARTESIAN_POINT ( 'NONE',  ( -5.044287576081563529, 45.27497882680665242, 92.45433879953097289 ) ) ;
#19245 = FACE_OUTER_BOUND ( 'NONE', #7383, .T. ) ;
#19246 = CARTESIAN_POINT ( 'NONE',  ( 6.960009239587057195, 50.34721145179211987, 76.80946857459053945 ) ) ;
#19247 = DIRECTION ( 'NONE',  ( -0.4999999999999983347, -0.8660254037844395958, 0.000000000000000000 ) ) ;
#19248 = CIRCLE ( 'NONE', #1590, 4.200000000000001066 ) ;
#19249 = ORIENTED_EDGE ( 'NONE', *, *, #20873, .F. ) ;
#19250 = CARTESIAN_POINT ( 'NONE',  ( -5.324466712459397399, 37.54042977870726361, 79.49842882144521639 ) ) ;
#19251 = CARTESIAN_POINT ( 'NONE',  ( 31.03948732994507864, 36.35905713404685002, 78.30433879953099563 ) ) ;
#19252 = CARTESIAN_POINT ( 'NONE',  ( -3.258387175647450729, 36.88553430894260998, 77.52493936945022313 ) ) ;
#19253 = ORIENTED_EDGE ( 'NONE', *, *, #15742, .T. ) ;
#19254 = CARTESIAN_POINT ( 'NONE',  ( 5.076572431691916520, 37.34329067111212197, 76.96022115247204454 ) ) ;
#19255 = EDGE_CURVE ( 'NONE', #9748, #13579, #637, .T. ) ;
#19256 = LINE ( 'NONE', #13311, #1333 ) ;
#19257 = ORIENTED_EDGE ( 'NONE', *, *, #10784, .F. ) ;
#19258 = CARTESIAN_POINT ( 'NONE',  ( 6.442019222303663639, 38.49630386955294625, 76.41040896618429201 ) ) ;
#19259 = AXIS2_PLACEMENT_3D ( 'NONE', #19888, #11308, #115 ) ;
#19260 = CARTESIAN_POINT ( 'NONE',  ( 8.911238338503892464, 41.50127112110217809, 78.09303657357962436 ) ) ;
#19261 = CARTESIAN_POINT ( 'NONE',  ( 5.679435644259863913, 37.95138956464963087, 78.36972961004526894 ) ) ;
#19262 = PRESENTATION_STYLE_ASSIGNMENT (( #17568 ) ) ;
#19263 = EDGE_CURVE ( 'NONE', #6443, #8901, #10128, .T. ) ;
#19264 = CARTESIAN_POINT ( 'NONE',  ( 8.124283007755586539, 44.40224511508533567, 72.45433879953087342 ) ) ;
#19265 = ORIENTED_EDGE ( 'NONE', *, *, #20113, .F. ) ;
#19266 = DIRECTION ( 'NONE',  ( -1.111814006898795283E-16, 5.922860397471810542E-17, -1.000000000000000000 ) ) ;
#19267 = ORIENTED_EDGE ( 'NONE', *, *, #19907, .F. ) ;
#19268 = DIRECTION ( 'NONE',  ( 1.402518428993831676E-16, -1.000000000000000000, 0.000000000000000000 ) ) ;
#19269 = CARTESIAN_POINT ( 'NONE',  ( -6.907938484555407044, 47.63351044088310005, 78.83514460925654532 ) ) ;
#19270 = VECTOR ( 'NONE', #10956, 1000.000000000000000 ) ;
#19271 = CARTESIAN_POINT ( 'NONE',  ( -7.631668735006648774, 47.47423462861603127, 78.95249617671795761 ) ) ;
#19272 = CARTESIAN_POINT ( 'NONE',  ( -5.486992102393413617, 39.49954625374182626, 72.45433879953085921 ) ) ;
#19273 = DIRECTION ( 'NONE',  ( -0.5941461771851692664, -0.8043570849667761591, -2.357623395011396791E-16 ) ) ;
#19274 = EDGE_CURVE ( 'NONE', #13986, #2342, #16608, .T. ) ;
#19275 =( GEOMETRIC_REPRESENTATION_CONTEXT ( 3 ) GLOBAL_UNCERTAINTY_ASSIGNED_CONTEXT ( ( #15131 ) ) GLOBAL_UNIT_ASSIGNED_CONTEXT ( ( #93, #16168, #3384 ) ) REPRESENTATION_CONTEXT ( 'NONE', 'WORKASPACE' ) );
#19276 = ORIENTED_EDGE ( 'NONE', *, *, #4301, .T. ) ;
#19277 = CARTESIAN_POINT ( 'NONE',  ( 8.230676153864024513, 41.36595300535771713, 76.07212865946658553 ) ) ;
#19278 = ORIENTED_EDGE ( 'NONE', *, *, #11326, .T. ) ;
#19279 = CARTESIAN_POINT ( 'NONE',  ( -3.653968934160817916, 51.07407364116832582, 75.42336258079946276 ) ) ;
#19280 = CARTESIAN_POINT ( 'NONE',  ( -5.784195910403845176, 44.99242805365518194, 93.53933880123797451 ) ) ;
#19281 = CARTESIAN_POINT ( 'NONE',  ( 4.100190290135135029, 51.54036911970691648, 75.45433879953088763 ) ) ;
#19282 = ORIENTED_EDGE ( 'NONE', *, *, #1413, .F. ) ;
#19283 = CARTESIAN_POINT ( 'NONE',  ( 2.064441844012933736, 52.21584861674933364, 77.34591136093878561 ) ) ;
#19284 = CARTESIAN_POINT ( 'NONE',  ( -1.077846259693497899, 47.82824192744436687, 85.55433879953100984 ) ) ;
#19285 = VECTOR ( 'NONE', #266, 1000.000000000000000 ) ;
#19286 = CARTESIAN_POINT ( 'NONE',  ( -4.559776018715442802, 36.97558356685869541, 78.86760481232144571 ) ) ;
#19287 = CARTESIAN_POINT ( 'NONE',  ( -4.541431855014749885, 51.35970071229581180, 78.93463757479271692 ) ) ;
#19288 = CARTESIAN_POINT ( 'NONE',  ( 5.074465183246152478, 37.34623967253333632, 77.43080938776617472 ) ) ;
#19289 = ORIENTED_EDGE ( 'NONE', *, *, #19409, .T. ) ;
#19290 = CARTESIAN_POINT ( 'NONE',  ( -3.226449543290886179, 47.76606447477297479, 92.55433879953076826 ) ) ;
#19291 = CARTESIAN_POINT ( 'NONE',  ( 0.3478318340824160249, 52.36035231526901157, 77.07067603543953282 ) ) ;
#19292 = VERTEX_POINT ( 'NONE', #19889 ) ;
#19293 = CARTESIAN_POINT ( 'NONE',  ( 4.401043237957516396, 51.32340155052948916, 77.79664654212120922 ) ) ;
#19294 = DIRECTION ( 'NONE',  ( -1.402518428993831183E-16, 1.000000000000000000, -3.469446951953617640E-16 ) ) ;
#19295 = CARTESIAN_POINT ( 'NONE',  ( -5.835808111729286374, 50.43478682938704338, 76.54939005541714891 ) ) ;
#19296 = CARTESIAN_POINT ( 'NONE',  ( -3.628867371436363953, 48.69222599884265179, 93.73558879782397923 ) ) ;
#19297 = CARTESIAN_POINT ( 'NONE',  ( -4.812088799398938299, 42.22067586467031930, 91.31371379782397923 ) ) ;
#19298 = DIRECTION ( 'NONE',  ( 1.000000000000000000, 1.402518428993842030E-16, 3.154042683594179047E-15 ) ) ;
#19299 = AXIS2_PLACEMENT_3D ( 'NONE', #10178, #11464, #11360 ) ;
#19300 = CARTESIAN_POINT ( 'NONE',  ( -3.673304938980983092, 36.32078308949211021, 77.52205638859560111 ) ) ;
#19301 = VERTEX_POINT ( 'NONE', #15121 ) ;
#19302 = CARTESIAN_POINT ( 'NONE',  ( -7.150937614292242728, 47.05418374649208602, 77.98057391402217320 ) ) ;
#19303 = ORIENTED_EDGE ( 'NONE', *, *, #5316, .T. ) ;
#19304 = DIRECTION ( 'NONE',  ( -0.000000000000000000, -0.000000000000000000, -1.000000000000000000 ) ) ;
#19305 = DIRECTION ( 'NONE',  ( -1.402518428993831183E-16, 1.000000000000000000, -3.469446951953617640E-16 ) ) ;
#19306 = CARTESIAN_POINT ( 'NONE',  ( 8.239900386529042109, 41.85364674066097024, 75.36311794487049553 ) ) ;
#19307 = CARTESIAN_POINT ( 'NONE',  ( -3.382060968773085374, 51.37355338276771022, 75.56522039652081446 ) ) ;
#19308 = EDGE_LOOP ( 'NONE', ( #13873, #7059, #19544, #12757, #3203, #15262, #18713, #14477 ) ) ;
#19309 = CARTESIAN_POINT ( 'NONE',  ( 0.5753667321910650445, 52.96202048236657589, 75.97198585835440099 ) ) ;
#19310 = ORIENTED_EDGE ( 'NONE', *, *, #9304, .T. ) ;
#19311 = CARTESIAN_POINT ( 'NONE',  ( -3.430514640876221044, 37.06627662345849217, 75.57130654555172100 ) ) ;
#19312 = DIRECTION ( 'NONE',  ( -0.5813877811926999595, 0.8136266022444382795, 5.636455622144657394E-17 ) ) ;
#19313 = CARTESIAN_POINT ( 'NONE',  ( -3.943187491250720544, 40.73580453397070755, 96.58621379953099506 ) ) ;
#19314 = ORIENTED_EDGE ( 'NONE', *, *, #14942, .T. ) ;
#19315 = CARTESIAN_POINT ( 'NONE',  ( -4.648332322150092288, 37.81575765971563641, 77.33253961758860839 ) ) ;
#19316 = CARTESIAN_POINT ( 'NONE',  ( 8.797519961583052606, 41.16044993131110630, 77.39661844205990349 ) ) ;
#19317 = CARTESIAN_POINT ( 'NONE',  ( -3.134114116279072881, 48.15229756555780227, 94.43871379953097289 ) ) ;
#19318 = AXIS2_PLACEMENT_3D ( 'NONE', #15576, #18866, #2691 ) ;
#19319 = ORIENTED_EDGE ( 'NONE', *, *, #3759, .F. ) ;
#19320 = DIRECTION ( 'NONE',  ( 1.000000000000000000, -1.193617070626243484E-16, 0.000000000000000000 ) ) ;
#19321 = DIRECTION ( 'NONE',  ( -0.3165065846431826535, -0.9485903129789529098, -2.188653791613874008E-16 ) ) ;
#19322 = CARTESIAN_POINT ( 'NONE',  ( -5.927888611570137911, 47.57933715648534445, 78.32492703482499508 ) ) ;
#19323 = CARTESIAN_POINT ( 'NONE',  ( -5.154188915835984375, 42.64120994080404614, 92.36746380123797451 ) ) ;
#19324 = EDGE_CURVE ( 'NONE', #13636, #20991, #19803, .T. ) ;
#19325 = DIRECTION ( 'NONE',  ( 1.402518428993831676E-16, -1.000000000000000000, 0.000000000000000000 ) ) ;
#19326 = CARTESIAN_POINT ( 'NONE',  ( 0.3837416960959899037, 52.96765485758538006, 77.02254451525793399 ) ) ;
#19327 = PLANE ( 'NONE',  #3703 ) ;
#19328 = VECTOR ( 'NONE', #15802, 1000.000000000000000 ) ;
#19329 = CARTESIAN_POINT ( 'NONE',  ( -3.981178359372548492, 46.76218137147973408, 92.91433880294496817 ) ) ;
#19330 = ORIENTED_EDGE ( 'NONE', *, *, #3983, .F. ) ;
#19331 = PLANE ( 'NONE',  #7795 ) ;
#19332 = DIRECTION ( 'NONE',  ( 0.000000000000000000, 0.000000000000000000, 1.000000000000000000 ) ) ;
#19333 = CARTESIAN_POINT ( 'NONE',  ( 8.496565932950701949, 40.25847161533236829, 79.21682452846883393 ) ) ;
#19334 = CARTESIAN_POINT ( 'NONE',  ( 1.424503621124223907, 52.91627723061543520, 79.43677396536959634 ) ) ;
#19335 = ORIENTED_EDGE ( 'NONE', *, *, #18102, .T. ) ;
#19336 = VECTOR ( 'NONE', #4519, 1000.000000000000000 ) ;
#19337 = ADVANCED_FACE ( 'NONE', ( #11624, #10351 ), #10024, .T. ) ;
#19338 = EDGE_LOOP ( 'NONE', ( #2909, #5802, #13118, #12178 ) ) ;
#19339 = VECTOR ( 'NONE', #16603, 1000.000000000000000 ) ;
#19340 = CARTESIAN_POINT ( 'NONE',  ( -3.508281668750850013, 47.93162672320032414, 78.65179900065425045 ) ) ;
#19341 = LINE ( 'NONE', #293, #14861 ) ;
#19342 = CARTESIAN_POINT ( 'NONE',  ( 5.217094560277743653, 37.43916672944678936, 77.75463208902168333 ) ) ;
#19343 = CARTESIAN_POINT ( 'NONE',  ( 4.178949506638397260, 51.50167206575788015, 78.81223402306018500 ) ) ;
#19345 = EDGE_CURVE ( 'NONE', #4999, #15976, #11824, .T. ) ;
#19344 = CARTESIAN_POINT ( 'NONE',  ( -4.812088799398939187, 42.22067586467031930, 92.56371379782397923 ) ) ;
#19346 = CARTESIAN_POINT ( 'NONE',  ( -5.154188915835984375, 42.64120994080404614, 93.46121380123805977 ) ) ;
#19347 = AXIS2_PLACEMENT_3D ( 'NONE', #516, #13499, #18398 ) ;
#19348 = PLANE ( 'NONE',  #4981 ) ;
#19349 = CARTESIAN_POINT ( 'NONE',  ( 6.344124029066668058, 49.87730810044735108, 77.50555814853646552 ) ) ;
#19350 = CARTESIAN_POINT ( 'NONE',  ( 4.175402538145164044, 51.50343628508133520, 78.12271961989166869 ) ) ;
#19351 =( BOUNDED_SURFACE ( )  B_SPLINE_SURFACE ( 1, 2, ( 
 ( #1543, #4710, #15816, #17400, #4406, #6009, #2825, #11238, #7618, #18993, #20882, #16123, #14000, #17710, #7823, #2925, #9537, #6111, #12615, #3142, #1335, #6312, #9329, #19195, #12813, #14412, #10829, #7717, #11130, #14199, #16020, #14100, #20483, #5916, #9643, #19296, #9425, #12413, #18892, #4302, #11030, #20583, #19102, #17501, #4610, #1130, #17292, #2718, #10929, #9225, #17600, #15711, #12509, #3028, #15914, #1228, #20677, #12717, #4512, #6217, #14306 ),
 ( #20783, #1440, #7925, #19818, #9843, #11442, #19509, #48, #17914, #5240, #1647, #13033, #14929, #10162, #16644, #11756, #1860, #18023, #3552, #148, #6630, #18230, #16441, #351, #3337, #13238, #6840, #8447, #4822, #1760, #5134, #8242, #10056, #8130, #14515, #8028, #3650, #13347, #3444, #20981, #6415, #12924, #5028, #14622, #13131, #9741, #19403, #9958, #6734, #8345, #11344, #17813, #3238, #16222, #6527, #4921, #16331, #14727, #19716, #19606, #11547 ) ),
 .UNSPECIFIED., .F., .F., .F. ) 
 B_SPLINE_SURFACE_WITH_KNOTS ( ( 2, 2 ),
 ( 3, 2, 2, 2, 2, 2, 2, 2, 2, 2, 2, 2, 2, 2, 2, 2, 2, 2, 2, 2, 2, 2, 2, 2, 2, 2, 2, 2, 2, 2, 3 ),
 ( 0.000000000000000000, 1.000000000000000000 ),
 ( 0.000000000000000000, 0.03125000000000000000, 0.06250000000000000000, 0.09375000000000000000, 0.1250000000000000000, 0.1562500000000000000, 0.1875000000000000000, 0.2187500000000000000, 0.2500000000000000000, 0.2812500000000000000, 0.3125000000000000000, 0.3437500000000000000, 0.3750000000000000000, 0.4062500000000000000, 0.4375000000000000000, 0.4687500000000000000, 0.5000000000000000000, 0.5312500000000000000, 0.5625000000000000000, 0.5937500000000000000, 0.6250000000000000000, 0.6562500000000000000, 0.6875000000000000000, 0.7187500000000000000, 0.7500000000000000000, 0.7812500000000000000, 0.8125000000000000000, 0.8437500000000000000, 0.8750000000000000000, 0.9062500000000000000, 0.9200238603477419730 ),
 .UNSPECIFIED. ) 
 GEOMETRIC_REPRESENTATION_ITEM ( )  RATIONAL_B_SPLINE_SURFACE ( (
 ( 1.000000000000000000, 0.9238795325112867385, 1.000000000000000000, 0.9238795325112867385, 1.000000000000000000, 0.9238795325112867385, 1.000000000000000000, 0.9238795325112867385, 1.000000000000000000, 0.9238795325112867385, 1.000000000000000000, 0.9238795325112867385, 1.000000000000000000, 0.9238795325112867385, 1.000000000000000000, 0.9238795325112867385, 1.000000000000000000, 0.9238795325112867385, 1.000000000000000000, 0.9238795325112867385, 1.000000000000000000, 0.9238795325112867385, 1.000000000000000000, 0.9238795325112867385, 1.000000000000000000, 0.9238795325112867385, 1.000000000000000000, 0.9238795325112867385, 1.000000000000000000, 0.9238795325112867385, 1.000000000000000000, 0.9238795325112867385, 1.000000000000000000, 0.9238795325112867385, 1.000000000000000000, 0.9238795325112867385, 1.000000000000000000, 0.9238795325112867385, 1.000000000000000000, 0.9238795325112867385, 1.000000000000000000, 0.9238795325112867385, 1.000000000000000000, 0.9238795325112867385, 1.000000000000000000, 0.9238795325112867385, 1.000000000000000000, 0.9238795325112867385, 1.000000000000000000, 0.9238795325112867385, 1.000000000000000000, 0.9238795325112867385, 1.000000000000000000, 0.9238795325112867385, 1.000000000000000000, 0.9238795325112867385, 1.000000000000000000, 0.9238795325112867385, 1.000000000000000000, 0.9664488739585801458, 0.9624739734918166256),
 ( 1.000000000000000000, 0.9238795325112867385, 1.000000000000000000, 0.9238795325112867385, 1.000000000000000000, 0.9238795325112867385, 1.000000000000000000, 0.9238795325112867385, 1.000000000000000000, 0.9238795325112867385, 1.000000000000000000, 0.9238795325112867385, 1.000000000000000000, 0.9238795325112867385, 1.000000000000000000, 0.9238795325112867385, 1.000000000000000000, 0.9238795325112867385, 1.000000000000000000, 0.9238795325112867385, 1.000000000000000000, 0.9238795325112867385, 1.000000000000000000, 0.9238795325112867385, 1.000000000000000000, 0.9238795325112867385, 1.000000000000000000, 0.9238795325112867385, 1.000000000000000000, 0.9238795325112867385, 1.000000000000000000, 0.9238795325112867385, 1.000000000000000000, 0.9238795325112867385, 1.000000000000000000, 0.9238795325112867385, 1.000000000000000000, 0.9238795325112867385, 1.000000000000000000, 0.9238795325112867385, 1.000000000000000000, 0.9238795325112867385, 1.000000000000000000, 0.9238795325112867385, 1.000000000000000000, 0.9238795325112867385, 1.000000000000000000, 0.9238795325112867385, 1.000000000000000000, 0.9238795325112867385, 1.000000000000000000, 0.9238795325112867385, 1.000000000000000000, 0.9238795325112867385, 1.000000000000000000, 0.9238795325112867385, 1.000000000000000000, 0.9238795325112867385, 1.000000000000000000, 0.9664488739585801458, 0.9624739734918166256) ) ) 
 REPRESENTATION_ITEM ( '' )  SURFACE ( )  );
#19352 = EDGE_CURVE ( 'NONE', #531, #14061, #4144, .T. ) ;
#19353 = VECTOR ( 'NONE', #11025, 1000.000000000000000 ) ;
#19354 = ORIENTED_EDGE ( 'NONE', *, *, #9776, .T. ) ;
#19355 = FACE_OUTER_BOUND ( 'NONE', #4606, .T. ) ;
#19356 = CARTESIAN_POINT ( 'NONE',  ( 5.497743849324332466, 37.64424434608246628, 76.58742703482498371 ) ) ;
#19357 = EDGE_CURVE ( 'NONE', #11321, #10416, #14044, .T. ) ;
#19358 = CARTESIAN_POINT ( 'NONE',  ( 5.262496838921983056, 50.85316300622503860, 78.84209982136016492 ) ) ;
#19359 = VECTOR ( 'NONE', #16510, 1000.000000000000114 ) ;
#19360 = VECTOR ( 'NONE', #4421, 1000.000000000000000 ) ;
#19361 = DIRECTION ( 'NONE',  ( -0.9534635866061452747, -0.3015081906286225522, -2.009271279954815797E-16 ) ) ;
#19362 = CARTESIAN_POINT ( 'NONE',  ( 8.390845173051939554, 39.94161979111582639, 76.38443001783366526 ) ) ;
#19363 = ORIENTED_EDGE ( 'NONE', *, *, #9256, .T. ) ;
#19365 = PRESENTATION_LAYER_ASSIGNMENT (  '', '', ( #6456 ) ) ;
#19364 = CARTESIAN_POINT ( 'NONE',  ( 6.582016959483238949, 37.67656554461878926, 75.62429547252081363 ) ) ;
#19366 = CARTESIAN_POINT ( 'NONE',  ( 5.561379608955574483, 51.38032281970146897, 76.90580938776616904 ) ) ;
#19367 = LINE ( 'NONE', #11307, #15865 ) ;
#19368 = FACE_OUTER_BOUND ( 'NONE', #1127, .T. ) ;
#19369 = CARTESIAN_POINT ( 'NONE',  ( 5.381183826744221577, 45.53750893733308658, 92.45433879953098710 ) ) ;
#19370 = ORIENTED_EDGE ( 'NONE', *, *, #2813, .F. ) ;
#19371 = CARTESIAN_POINT ( 'NONE',  ( 8.936058775400656629, 41.57565954506093675, 76.08336210994360727 ) ) ;
#19372 = VERTEX_POINT ( 'NONE', #20623 ) ;
#19373 = CARTESIAN_POINT ( 'NONE',  ( 3.460444912181559474, 49.25145096859824889, 94.24246380123798872 ) ) ;
#19374 = AXIS2_PLACEMENT_3D ( 'NONE', #18389, #2121, #510 ) ;
#19375 = EDGE_CURVE ( 'NONE', #19551, #15771, #4242, .T. ) ;
#19376 = CARTESIAN_POINT ( 'NONE',  ( 4.394343283833276992, 39.11584570990505938, 91.35183880123798872 ) ) ;
#19377 = CARTESIAN_POINT ( 'NONE',  ( 0.3802186396914607469, 52.36096666664144550, 76.04253254076220969 ) ) ;
#19378 = CARTESIAN_POINT ( 'NONE',  ( 0.8377421044266871730, 51.35991668224300355, 76.48963291717792856 ) ) ;
#19379 = EDGE_CURVE ( 'NONE', #14271, #5223, #4051, .T. ) ;
#19380 = CARTESIAN_POINT ( 'NONE',  ( -7.889981766995627588, 41.56529470657834935, 78.93438826577718714 ) ) ;
#19381 = CIRCLE ( 'NONE', #10237, 3.999999999999996447 ) ;
#19382 = ORIENTED_EDGE ( 'NONE', *, *, #13064, .F. ) ;
#19383 = ADVANCED_FACE ( 'NONE', ( #960 ), #8950, .F. ) ;
#19384 = DIRECTION ( 'NONE',  ( -0.3165065846431827645, -0.9485903129789529098, 0.000000000000000000 ) ) ;
#19385 = EDGE_CURVE ( 'NONE', #2251, #12080, #7557, .T. ) ;
#19386 = EDGE_LOOP ( 'NONE', ( #1514, #7508, #12595, #9806 ) ) ;
#19387 = DIRECTION ( 'NONE',  ( -1.779391786395883536E-16, -5.922860397471805611E-17, 1.000000000000000000 ) ) ;
#19388 = CARTESIAN_POINT ( 'NONE',  ( 6.828503391016846891, 43.33193468930419101, 91.66433880123796030 ) ) ;
#19389 = CARTESIAN_POINT ( 'NONE',  ( -3.944959226007136888, 38.51060946023304865, 77.05433879953086773 ) ) ;
#19390 = EDGE_LOOP ( 'NONE', ( #70, #19420, #3973, #14054 ) ) ;
#19391 = CARTESIAN_POINT ( 'NONE',  ( 1.765050448036873831, 52.26768315785694341, 76.95678149889430131 ) ) ;
#19392 = CARTESIAN_POINT ( 'NONE',  ( -5.522333806888468644, 37.68658623078928116, 79.43312132436682305 ) ) ;
#19393 = CARTESIAN_POINT ( 'NONE',  ( 4.208451567978901409, 39.70256125636758071, 92.55433879953093879 ) ) ;
#19394 = CARTESIAN_POINT ( 'NONE',  ( 5.292744349709337826, 50.82411692241547740, 75.98863418974025308 ) ) ;
#19395 = CARTESIAN_POINT ( 'NONE',  ( 5.430298293217690642, 36.85358955281711246, 77.55899030588862786 ) ) ;
#19396 = ORIENTED_EDGE ( 'NONE', *, *, #19982, .F. ) ;
#19397 = CYLINDRICAL_SURFACE ( 'NONE', #18005, 4.200000000000001954 ) ;
#19398 = CARTESIAN_POINT ( 'NONE',  ( 9.273778039597953438, 45.67340037358405169, 78.74919174070734584 ) ) ;
#19399 = VERTEX_POINT ( 'NONE', #20424 ) ;
#19400 = FACE_OUTER_BOUND ( 'NONE', #17570, .T. ) ;
#19401 = FACE_OUTER_BOUND ( 'NONE', #17893, .T. ) ;
#19402 = CARTESIAN_POINT ( 'NONE',  ( -5.374794079232331434, 49.84443499592996574, 76.21531548689122815 ) ) ;
#19403 = CARTESIAN_POINT ( 'NONE',  ( 5.220616844236030119, 45.87228208810806507, 94.98558879611698558 ) ) ;
#19404 = CARTESIAN_POINT ( 'NONE',  ( 4.673174852049363004, 39.63213674411673537, 91.70433879782397923 ) ) ;
#19405 = CIRCLE ( 'NONE', #15692, 1.399999999999995026 ) ;
#19406 = CARTESIAN_POINT ( 'NONE',  ( 6.545534159973747990, 50.65336749702785113, 77.68963291717794561 ) ) ;
#19407 = CARTESIAN_POINT ( 'NONE',  ( 5.573315379359557120, 50.61687040490333089, 76.21496574784163158 ) ) ;
#19408 = ORIENTED_EDGE ( 'NONE', *, *, #6387, .F. ) ;
#19409 = EDGE_CURVE ( 'NONE', #2631, #6196, #7232, .T. ) ;
#19410 = CARTESIAN_POINT ( 'NONE',  ( 1.934299931914925441, 52.20294349804878919, 79.09265199143256098 ) ) ;
#19411 = CARTESIAN_POINT ( 'NONE',  ( -3.499411194686691040, 37.10634979067736339, 77.70026928173652436 ) ) ;
#19412 = ORIENTED_EDGE ( 'NONE', *, *, #4784, .T. ) ;
#19413 = DIRECTION ( 'NONE',  ( 0.4999999999999981126, -0.8660254037844397068, -0.000000000000000000 ) ) ;
#19414 = FACE_OUTER_BOUND ( 'NONE', #11948, .T. ) ;
#19415 = DIRECTION ( 'NONE',  ( 2.043266227890062685E-16, 0.7071067811865451302, -0.7071067811865500152 ) ) ;
#19416 = CARTESIAN_POINT ( 'NONE',  ( 7.975192330168971111, 41.06029990298387844, 79.49103220525971381 ) ) ;
#19417 = EDGE_LOOP ( 'NONE', ( #8258, #5051, #19044, #15484 ) ) ;
#19418 = CARTESIAN_POINT ( 'NONE',  ( 2.263363662449358493, 49.77488197367694767, 94.44231768333818877 ) ) ;
#19419 = FACE_OUTER_BOUND ( 'NONE', #15265, .T. ) ;
#19420 = ORIENTED_EDGE ( 'NONE', *, *, #10805, .F. ) ;
#19421 = VECTOR ( 'NONE', #17229, 1000.000000000000000 ) ;
#19422 = CARTESIAN_POINT ( 'NONE',  ( -1.117719678584871090, 36.12782917792895176, 76.86610350541323555 ) ) ;
#19423 = PLANE ( 'NONE',  #4717 ) ;
#19424 = CARTESIAN_POINT ( 'NONE',  ( 5.025485839985549319, 41.56218137147963887, 95.72683879953099506 ) ) ;
#19425 = AXIS2_PLACEMENT_3D ( 'NONE', #20920, #6669, #14659 ) ;
#19426 = ORIENTED_EDGE ( 'NONE', *, *, #9501, .T. ) ;
#19427 = CARTESIAN_POINT ( 'NONE',  ( -4.900087432442492563, 37.22695789959892920, 77.32461911834714385 ) ) ;
#19428 = CARTESIAN_POINT ( 'NONE',  ( 8.211361072458180033, 41.32375023436543415, 77.14698585835439815 ) ) ;
#19429 = CARTESIAN_POINT ( 'NONE',  ( 5.053692675489762642, 42.04909006277621586, 92.64183879953097289 ) ) ;
#19430 = ORIENTED_EDGE ( 'NONE', *, *, #13438, .T. ) ;
#19431 = CARTESIAN_POINT ( 'NONE',  ( -4.804644443005473775, 51.17161863374556674, 76.44036821129557779 ) ) ;
#19432 = CARTESIAN_POINT ( 'NONE',  ( -1.483269432489140005, 51.49895708687498086, 72.45432679953087529 ) ) ;
#19433 = CARTESIAN_POINT ( 'NONE',  ( 2.522153740306507963, 49.16218137147969003, 66.55433879953099563 ) ) ;
#19434 = CARTESIAN_POINT ( 'NONE',  ( -5.387797286270752828, 50.75491896253648605, 75.54244301425877950 ) ) ;
#19435 = CARTESIAN_POINT ( 'NONE',  ( -4.514796398449106185, 37.69153629922272586, 76.06698014943201258 ) ) ;
#19436 = AXIS2_PLACEMENT_3D ( 'NONE', #19845, #3888, #15288 ) ;
#19437 = CARTESIAN_POINT ( 'NONE',  ( -7.367656984315425817, 48.05973018190410073, 78.78375056423675460 ) ) ;
#19438 = LINE ( 'NONE', #1369, #15283 ) ;
#19439 = VECTOR ( 'NONE', #3719, 1000.000000000000000 ) ;
#19440 = CARTESIAN_POINT ( 'NONE',  ( 8.385768451058924100, 39.92640453324153071, 77.75090705316073070 ) ) ;
#19441 = VERTEX_POINT ( 'NONE', #4347 ) ;
#19442 = CARTESIAN_POINT ( 'NONE',  ( 5.561379608955574483, 51.38032281970146897, 76.90580938776616904 ) ) ;
#19443 = CARTESIAN_POINT ( 'NONE',  ( 8.561605920521204283, 42.81781863465402438, 75.72637824826109920 ) ) ;
#19444 = CARTESIAN_POINT ( 'NONE',  ( 0.8431461159794668703, 52.35589634692465211, 76.25677998097611976 ) ) ;
#19445 = ORIENTED_EDGE ( 'NONE', *, *, #18627, .T. ) ;
#19446 = ORIENTED_EDGE ( 'NONE', *, *, #3381, .T. ) ;
#19447 = EDGE_CURVE ( 'NONE', #16624, #4579, #15438, .T. ) ;
#19448 = AXIS2_PLACEMENT_3D ( 'NONE', #15329, #2023, #2232 ) ;
#19449 = AXIS2_PLACEMENT_3D ( 'NONE', #10418, #16786, #8918 ) ;
#19450 = CARTESIAN_POINT ( 'NONE',  ( 7.705497127814430414, 40.20743238930150198, 76.12097142257781002 ) ) ;
#19451 = CARTESIAN_POINT ( 'NONE',  ( -1.477846259693490705, 50.16218137147969713, 59.55433879953099563 ) ) ;
#19452 = CARTESIAN_POINT ( 'NONE',  ( 0.5221537403065013017, 44.16218137147968292, 76.86610350541323555 ) ) ;
#19453 = CARTESIAN_POINT ( 'NONE',  ( 8.722153740306517022, 44.16218137147969003, 54.55433879953099563 ) ) ;
#19454 = CARTESIAN_POINT ( 'NONE',  ( -1.419351766502867873, 49.49642391118513274, 93.50121379782397923 ) ) ;
#19455 = CARTESIAN_POINT ( 'NONE',  ( 5.848951923618479931, 37.15274410921379911, 76.58742703482498371 ) ) ;
#19456 = PLANE ( 'NONE',  #9764 ) ;
#19457 = DIRECTION ( 'NONE',  ( 3.893792155548169402E-16, 7.183611964723547524E-17, -1.000000000000000000 ) ) ;
#19458 = LINE ( 'NONE', #10010, #275 ) ;
#19459 = EDGE_CURVE ( 'NONE', #19585, #11503, #8844, .T. ) ;
#19460 = CARTESIAN_POINT ( 'NONE',  ( 1.352400422481993658, 50.46853102219002096, 91.82058880123801714 ) ) ;
#19461 = ORIENTED_EDGE ( 'NONE', *, *, #7004, .T. ) ;
#19462 = DIRECTION ( 'NONE',  ( 1.540237394707284220E-16, 1.793354297423764243E-16, -1.000000000000000000 ) ) ;
#19463 = VECTOR ( 'NONE', #14813, 1000.000000000000114 ) ;
#19464 = CARTESIAN_POINT ( 'NONE',  ( 8.924621998940734713, 41.54138280047497744, 78.88894238123772595 ) ) ;
#19465 = CARTESIAN_POINT ( 'NONE',  ( 5.241745939415380917, 50.86780957443158258, 78.63052193300478621 ) ) ;
#19466 = CARTESIAN_POINT ( 'NONE',  ( 8.941883057029242465, 41.59311528658734147, 77.39218765127517941 ) ) ;
#19467 = CARTESIAN_POINT ( 'NONE',  ( 9.242846470233811118, 42.49512172872434945, 77.95057265855270145 ) ) ;
#19468 = VERTEX_POINT ( 'NONE', #2660 ) ;
#19469 = CARTESIAN_POINT ( 'NONE',  ( -0.3247337541324620269, 52.97381866229035552, 75.52908203832478762 ) ) ;
#19470 = CARTESIAN_POINT ( 'NONE',  ( 0.5221481216947261306, 52.96836594783012941, 79.54816788430672148 ) ) ;
#19471 = CARTESIAN_POINT ( 'NONE',  ( 6.716472115211415961, 37.77264227618470471, 78.07897440853361104 ) ) ;
#19472 = CARTESIAN_POINT ( 'NONE',  ( 11.22215374030650281, 42.96218137147968008, 61.80715055817104542 ) ) ;
#19473 = CARTESIAN_POINT ( 'NONE',  ( 7.753636062665578699, 48.02814353133176439, 72.45433879953087342 ) ) ;
#19474 = EDGE_LOOP ( 'NONE', ( #20897, #18788, #12968, #7799 ) ) ;
#19475 =( BOUNDED_CURVE ( )  B_SPLINE_CURVE ( 3, ( #19284, #8015, #9318, #6301 ),
 .UNSPECIFIED., .F., .T. ) 
 B_SPLINE_CURVE_WITH_KNOTS ( ( 4, 4 ),
 ( 1.982313172862385509, 2.094395102393197927 ),
 .UNSPECIFIED. ) 
 CURVE ( )  GEOMETRIC_REPRESENTATION_ITEM ( )  RATIONAL_B_SPLINE_CURVE ( ( 1.000000000000000000, 0.9989534107080366709, 0.9989534107080366709, 1.000000000000000000 ) ) 
 REPRESENTATION_ITEM ( '' )  );
#19476 = DIRECTION ( 'NONE',  ( -1.402518428993831183E-16, 1.000000000000000000, -3.469446951953617640E-16 ) ) ;
#19477 = VECTOR ( 'NONE', #9374, 1000.000000000000000 ) ;
#19478 = ORIENTED_EDGE ( 'NONE', *, *, #1275, .F. ) ;
#19479 = CARTESIAN_POINT ( 'NONE',  ( 3.122153740306552905, 48.66551347115873227, 95.10183880294498238 ) ) ;
#19480 = CARTESIAN_POINT ( 'NONE',  ( 11.22215374030649926, 42.76218137147968434, 77.80433879953099563 ) ) ;
#19481 = CARTESIAN_POINT ( 'NONE',  ( 5.008975552073978932, 51.78836144432716537, 77.68963291717794561 ) ) ;
#19482 = EDGE_CURVE ( 'NONE', #972, #10052, #20309, .T. ) ;
#19483 = CARTESIAN_POINT ( 'NONE',  ( -7.293281983365068832, 41.70860050496550997, 78.93589458924091673 ) ) ;
#19484 = CARTESIAN_POINT ( 'NONE',  ( 8.124283007755586539, 44.40224511508533567, 75.45433879953087342 ) ) ;
#19485 = ORIENTED_EDGE ( 'NONE', *, *, #13749, .F. ) ;
#19486 = CARTESIAN_POINT ( 'NONE',  ( 0.5221537403065010796, 44.16218137147969003, 92.55433879953098142 ) ) ;
#19487 = VERTEX_POINT ( 'NONE', #14140 ) ;
#19488 = VECTOR ( 'NONE', #17998, 1000.000000000000000 ) ;
#19489 = CARTESIAN_POINT ( 'NONE',  ( -3.055882809522131094, 36.78399362325244937, 72.45433879953085921 ) ) ;
#19490 = CARTESIAN_POINT ( 'NONE',  ( -3.350035803220276609, 49.20851703305431357, 92.13308880123798872 ) ) ;
#19491 = CARTESIAN_POINT ( 'NONE',  ( 5.611423337425062385, 41.22389019960463230, 93.92996380123798872 ) ) ;
#19492 = VERTEX_POINT ( 'NONE', #9162 ) ;
#19493 = EDGE_CURVE ( 'NONE', #16288, #5383, #13730, .T. ) ;
#19494 = CARTESIAN_POINT ( 'NONE',  ( 2.115041367457929589, 52.20598078514408513, 77.84551527011910821 ) ) ;
#19495 = LINE ( 'NONE', #11643, #4832 ) ;
#19496 = CARTESIAN_POINT ( 'NONE',  ( 5.438522061964698118, 41.32291878214397940, 92.55433879953102405 ) ) ;
#19497 = FACE_OUTER_BOUND ( 'NONE', #2598, .T. ) ;
#19498 = EDGE_CURVE ( 'NONE', #13415, #11839, #5635, .T. ) ;
#19499 = PLANE ( 'NONE',  #2805 ) ;
#19500 = ORIENTED_EDGE ( 'NONE', *, *, #5864, .T. ) ;
#19501 = CARTESIAN_POINT ( 'NONE',  ( -4.383473025373058718, 51.47257230871590394, 76.47051527011910821 ) ) ;
#19502 = DIRECTION ( 'NONE',  ( 1.000000000000000000, 0.000000000000000000, 0.000000000000000000 ) ) ;
#19503 = VERTEX_POINT ( 'NONE', #20527 ) ;
#19504 = CARTESIAN_POINT ( 'NONE',  ( 1.528832406012765377, 49.31710775539747260, 95.05433879953095300 ) ) ;
#19505 = CARTESIAN_POINT ( 'NONE',  ( -7.807343701989813312, 41.29925972579167137, 76.45513158819304067 ) ) ;
#19506 = EDGE_CURVE ( 'NONE', #14425, #8220, #7339, .T. ) ;
#19507 = EDGE_CURVE ( 'NONE', #9577, #597, #15763, .T. ) ;
#19508 = DIRECTION ( 'NONE',  ( -0.000000000000000000, -0.000000000000000000, 1.000000000000000000 ) ) ;
#19509 = CARTESIAN_POINT ( 'NONE',  ( -4.176309363623029292, 42.45208065485131499, 91.86058879611698558 ) ) ;
#19510 = FACE_OUTER_BOUND ( 'NONE', #20057, .T. ) ;
#19511 = ADVANCED_FACE ( 'NONE', ( #17645 ), #7975, .F. ) ;
#19512 = CARTESIAN_POINT ( 'NONE',  ( -3.677846259693482001, 44.16218137147969003, 54.55433879953099563 ) ) ;
#19513 = CARTESIAN_POINT ( 'NONE',  ( 5.631785411401764918, 36.99756487055721976, 77.76022115247205591 ) ) ;
#19514 = CARTESIAN_POINT ( 'NONE',  ( -7.154059339130676598, 47.04588606493869918, 75.45433879953087342 ) ) ;
#19515 = ORIENTED_EDGE ( 'NONE', *, *, #13239, .T. ) ;
#19516 = CARTESIAN_POINT ( 'NONE',  ( 1.515499286945060975, 52.95892085087707102, 79.40139704896512285 ) ) ;
#19517 = DIRECTION ( 'NONE',  ( -1.540237394707284220E-16, -1.793354297423764243E-16, 1.000000000000000000 ) ) ;
#19518 = EDGE_LOOP ( 'NONE', ( #11842, #9123, #13512, #16531 ) ) ;
#19519 = DIRECTION ( 'NONE',  ( 1.540237394707284220E-16, 1.793354297423764243E-16, -1.000000000000000000 ) ) ;
#19520 = CARTESIAN_POINT ( 'NONE',  ( 2.877538411150256437, 49.16070722497604351, 92.79646262933300704 ) ) ;
#19521 = CARTESIAN_POINT ( 'NONE',  ( 9.026706097321888222, 41.84733531941775198, 79.51559944055343010 ) ) ;
#19522 = ORIENTED_EDGE ( 'NONE', *, *, #1121, .T. ) ;
#19523 = CARTESIAN_POINT ( 'NONE',  ( -4.567115856812060670, 47.10047254335474065, 93.46121380123797451 ) ) ;
#19524 = CARTESIAN_POINT ( 'NONE',  ( 2.916646314871006229, 38.79555996194933698, 95.05433879953095300 ) ) ;
#19525 = EDGE_LOOP ( 'NONE', ( #16247, #16322, #19515, #18745 ) ) ;
#19526 = CARTESIAN_POINT ( 'NONE',  ( 0.5221537403064999694, 39.16218137147969003, 92.45433879953097289 ) ) ;
#19527 = CARTESIAN_POINT ( 'NONE',  ( 1.015734901122072875, 52.94862456227837555, 76.77344627088704954 ) ) ;
#19528 = CARTESIAN_POINT ( 'NONE',  ( -3.943187491250720544, 40.73580453397070755, 92.83621379953099506 ) ) ;
#19529 = ORIENTED_EDGE ( 'NONE', *, *, #14802, .T. ) ;
#19530 = CARTESIAN_POINT ( 'NONE',  ( -4.956093006374739041, 37.26832696102055564, 77.32892190166411694 ) ) ;
#19531 = DIRECTION ( 'NONE',  ( -1.402518428993831183E-16, 1.000000000000000000, -3.469446951953617640E-16 ) ) ;
#19532 = CARTESIAN_POINT ( 'NONE',  ( 2.635245049009969254, 48.69372030666295359, 92.95433879953098710 ) ) ;
#19533 = ORIENTED_EDGE ( 'NONE', *, *, #5592, .T. ) ;
#19534 = CARTESIAN_POINT ( 'NONE',  ( -7.841408665719470150, 41.42496028907581973, 78.93240061090689608 ) ) ;
#19535 = DIRECTION ( 'NONE',  ( 1.000000000000000000, 0.000000000000000000, -0.000000000000000000 ) ) ;
#19536 = CARTESIAN_POINT ( 'NONE',  ( 2.898327458951320157, 49.13991817717495536, 94.03907478705464484 ) ) ;
#19537 = EDGE_CURVE ( 'NONE', #13249, #8576, #6525, .T. ) ;
#19538 = DIRECTION ( 'NONE',  ( 1.000000000000000000, 0.000000000000000000, 0.000000000000000000 ) ) ;
#19539 = CARTESIAN_POINT ( 'NONE',  ( 6.467647404187965243, 50.71089930605690910, 75.49932683761802821 ) ) ;
#19540 = DIRECTION ( 'NONE',  ( 1.540237394707284220E-16, 1.793354297423764243E-16, -1.000000000000000000 ) ) ;
#19541 = CARTESIAN_POINT ( 'NONE',  ( -1.123656915330052408, 35.37488560990637865, 76.86610350541323555 ) ) ;
#19542 = CARTESIAN_POINT ( 'NONE',  ( 0.5221537403065019678, 44.16218137147968292, 72.45433879953087342 ) ) ;
#19543 = CARTESIAN_POINT ( 'NONE',  ( 7.676123242391161838, 40.16397087432461177, 78.01856368782078732 ) ) ;
#19544 = ORIENTED_EDGE ( 'NONE', *, *, #10554, .F. ) ;
#19545 = LINE ( 'NONE', #12961, #15636 ) ;
#19546 = CARTESIAN_POINT ( 'NONE',  ( -2.503296703960774305, 48.49064145155254124, 94.11279910766216972 ) ) ;
#19547 = DIRECTION ( 'NONE',  ( 1.193617070626243237E-16, 1.000000000000000000, 1.876284981264363171E-30 ) ) ;
#19548 = CARTESIAN_POINT ( 'NONE',  ( 2.108066629828172722, 52.81809899402443875, 78.56377684848334297 ) ) ;
#19549 = ORIENTED_EDGE ( 'NONE', *, *, #2550, .F. ) ;
#19550 = CARTESIAN_POINT ( 'NONE',  ( 10.77494014480653561, 42.96218137147968008, 74.20433879953100131 ) ) ;
#19551 = VERTEX_POINT ( 'NONE', #17859 ) ;
#19552 = DIRECTION ( 'NONE',  ( -1.000000000000000000, 3.304235192336774723E-15, 0.000000000000000000 ) ) ;
#19553 = DIRECTION ( 'NONE',  ( -0.000000000000000000, -0.000000000000000000, 1.000000000000000000 ) ) ;
#19554 = LINE ( 'NONE', #6787, #6876 ) ;
#19555 = CARTESIAN_POINT ( 'NONE',  ( -4.677846259693496656, 44.16218127507082158, 94.26911326394257173 ) ) ;
#19556 = PRODUCT_DEFINITION_SHAPE ( 'NONE', 'NONE',  #16133 ) ;
#19557 = CARTESIAN_POINT ( 'NONE',  ( -4.567115856812060670, 47.10047254335474065, 93.30496380123805977 ) ) ;
#19558 = CARTESIAN_POINT ( 'NONE',  ( 6.828109521384686076, 50.44464046038347504, 77.45110917081549928 ) ) ;
#19559 = CARTESIAN_POINT ( 'NONE',  ( -3.495392342740027303, 36.18936622140545012, 76.59109406773794149 ) ) ;
#19560 = CARTESIAN_POINT ( 'NONE',  ( -4.511001915486199110, 37.69419204354686315, 76.06675994099744287 ) ) ;
#19561 = CARTESIAN_POINT ( 'NONE',  ( -3.350035803220276609, 49.20851703305431357, 91.97683880123797451 ) ) ;
#19562 = ORIENTED_EDGE ( 'NONE', *, *, #12534, .T. ) ;
#19563 = CARTESIAN_POINT ( 'NONE',  ( -5.803682309770403336, 37.89440703645915676, 79.21211992218960063 ) ) ;
#19564 = CARTESIAN_POINT ( 'NONE',  ( -5.838428831739583380, 50.43291415881836315, 78.10580938776615767 ) ) ;
#19565 = CARTESIAN_POINT ( 'NONE',  ( 8.457937123238437493, 42.09516238501478824, 75.39874760587915148 ) ) ;
#19566 = LINE ( 'NONE', #8306, #18024 ) ;
#19567 = CARTESIAN_POINT ( 'NONE',  ( 8.509969478268430976, 40.29864289095467456, 75.64968528315669971 ) ) ;
#19568 = ORIENTED_EDGE ( 'NONE', *, *, #13724, .F. ) ;
#19569 = VERTEX_POINT ( 'NONE', #12862 ) ;
#19570 = CARTESIAN_POINT ( 'NONE',  ( 0.5981972045264781768, 52.96654101249860247, 75.36022115247205022 ) ) ;
#19571 = CARTESIAN_POINT ( 'NONE',  ( 0.5161363701343861798, 52.20597262174597120, 79.54816788430672148 ) ) ;
#19572 = CARTESIAN_POINT ( 'NONE',  ( 6.169334044264807915, 38.30145302496794812, 78.19824744938543404 ) ) ;
#19573 = CARTESIAN_POINT ( 'NONE',  ( 4.844805589496135489, 51.13093757591915534, 75.42224697063917915 ) ) ;
#19574 = DIRECTION ( 'NONE',  ( -1.540237394707284467E-16, -1.793354297423764243E-16, 1.000000000000000000 ) ) ;
#19575 = VERTEX_POINT ( 'NONE', #17450 ) ;
#19576 = CARTESIAN_POINT ( 'NONE',  ( 8.909863635552733641, 41.49715104914803021, 76.00786757613292366 ) ) ;
#19577 = VECTOR ( 'NONE', #1469, 1000.000000000000000 ) ;
#19578 = ORIENTED_EDGE ( 'NONE', *, *, #15039, .T. ) ;
#19579 = CARTESIAN_POINT ( 'NONE',  ( 2.043125170982144745, 38.48583871533720213, 92.52371380123798872 ) ) ;
#19580 = DIRECTION ( 'NONE',  ( -0.000000000000000000, -0.000000000000000000, 1.000000000000000000 ) ) ;
#19581 = FACE_OUTER_BOUND ( 'NONE', #18342, .T. ) ;
#19582 = CARTESIAN_POINT ( 'NONE',  ( 8.327750958825182792, 41.64958601982033315, 75.98936102326365472 ) ) ;
#19583 = EDGE_CURVE ( 'NONE', #8823, #15970, #4457, .T. ) ;
#19584 = LINE ( 'NONE', #5006, #6825 ) ;
#19585 = VERTEX_POINT ( 'NONE', #9475 ) ;
#19586 = EDGE_LOOP ( 'NONE', ( #7007, #7031, #18806, #14661 ) ) ;
#19587 = AXIS2_PLACEMENT_3D ( 'NONE', #11651, #18129, #671 ) ;
#19588 = CARTESIAN_POINT ( 'NONE',  ( -1.392380047608626770, 49.84925249003585179, 69.23980501161585721 ) ) ;
#19589 = DIRECTION ( 'NONE',  ( -1.540237394707284467E-16, -1.793354297423764243E-16, 1.000000000000000000 ) ) ;
#19590 = CARTESIAN_POINT ( 'NONE',  ( 26.43948732994508788, 36.35905713404684292, 76.90433879953101837 ) ) ;
#19591 =( BOUNDED_CURVE ( )  B_SPLINE_CURVE ( 3, ( #5346, #356, #16854, #10164 ),
 .UNSPECIFIED., .F., .T. ) 
 B_SPLINE_CURVE_WITH_KNOTS ( ( 4, 4 ),
 ( 4.662421992893787781, 4.819209660608428258 ),
 .UNSPECIFIED. ) 
 CURVE ( )  GEOMETRIC_REPRESENTATION_ITEM ( )  RATIONAL_B_SPLINE_CURVE ( ( 1.000000000000000000, 0.9979525178427032239, 0.9979525178427032239, 1.000000000000000000 ) ) 
 REPRESENTATION_ITEM ( '' )  );
#19592 = ORIENTED_EDGE ( 'NONE', *, *, #15429, .T. ) ;
#19593 = CARTESIAN_POINT ( 'NONE',  ( 8.228459776970742823, 41.35979042148017015, 77.86767600988038396 ) ) ;
#19594 = LINE ( 'NONE', #18011, #1806 ) ;
#19595 = LINE ( 'NONE', #9945, #9136 ) ;
#19596 = EDGE_CURVE ( 'NONE', #8000, #16102, #2875, .T. ) ;
#19597 = LINE ( 'NONE', #1750, #7449 ) ;
#19598 = FACE_OUTER_BOUND ( 'NONE', #3407, .T. ) ;
#19599 = ORIENTED_EDGE ( 'NONE', *, *, #6156, .T. ) ;
#19600 = PLANE ( 'NONE',  #3396 ) ;
#19601 = CARTESIAN_POINT ( 'NONE',  ( 2.035123479059381957, 36.10296785094195826, 76.86610350541323555 ) ) ;
#19602 = EDGE_LOOP ( 'NONE', ( #9935, #5809, #17407, #17981, #7631 ) ) ;
#19603 = CARTESIAN_POINT ( 'NONE',  ( 4.160801005917750039, 51.50085880978985386, 78.17666347917207759 ) ) ;
#19604 = CARTESIAN_POINT ( 'NONE',  ( -7.423027804938098662, 40.08393216593763952, 78.33343394419354411 ) ) ;
#19605 = CARTESIAN_POINT ( 'NONE',  ( 4.539372959821318609, 52.13523796247791608, 76.58963291717793709 ) ) ;
#19606 = CARTESIAN_POINT ( 'NONE',  ( 3.052270314075706814, 39.76217963117571230, 95.95600669793734028 ) ) ;
#19607 = CARTESIAN_POINT ( 'NONE',  ( 2.463659247115867146, 38.82793883177424732, 92.87621379782399345 ) ) ;
#19608 = LINE ( 'NONE', #18968, #10960 ) ;
#19610 = EDGE_CURVE ( 'NONE', #10073, #9723, #1545, .T. ) ;
#19609 = CARTESIAN_POINT ( 'NONE',  ( 24.43948732994508077, 36.35905713404685002, 76.90433879953101837 ) ) ;
#19611 = EDGE_CURVE ( 'NONE', #10155, #12110, #19048, .T. ) ;
#19612 = CARTESIAN_POINT ( 'NONE',  ( 5.921589662822362321, 51.11425016305613411, 76.13071926429850578 ) ) ;
#19613 = VERTEX_POINT ( 'NONE', #15857 ) ;
#19614 = CARTESIAN_POINT ( 'NONE',  ( 1.368073678578153762, 52.96008335597884553, 79.45495304649941204 ) ) ;
#19615 = LINE ( 'NONE', #16338, #18053 ) ;
#19616 = VECTOR ( 'NONE', #20100, 1000.000000000000000 ) ;
#19617 = ORIENTED_EDGE ( 'NONE', *, *, #7380, .T. ) ;
#19618 = LINE ( 'NONE', #20031, #20037 ) ;
#19619 = EDGE_CURVE ( 'NONE', #9302, #19082, #13978, .T. ) ;
#19620 = CARTESIAN_POINT ( 'NONE',  ( 31.22215374030650281, 42.96218137147968008, 73.80433879953100984 ) ) ;
#19621 = CARTESIAN_POINT ( 'NONE',  ( 8.990918003704509331, 41.74007613249212767, 79.53018343098241871 ) ) ;
#19622 = VERTEX_POINT ( 'NONE', #20833 ) ;
#19623 = CARTESIAN_POINT ( 'NONE',  ( -2.416137431568557314, 39.07291177436112406, 96.27371380123797451 ) ) ;
#19624 = CARTESIAN_POINT ( 'NONE',  ( -5.251100579623900977, 37.48623717174978509, 75.42164981362142839 ) ) ;
#19625 = ORIENTED_EDGE ( 'NONE', *, *, #4652, .T. ) ;
#19626 = VECTOR ( 'NONE', #9243, 1000.000000000000000 ) ;
#19627 = LINE ( 'NONE', #17828, #7417 ) ;
#19628 = CARTESIAN_POINT ( 'NONE',  ( 0.8006569122482152245, 52.95806462237449352, 76.79591147939019891 ) ) ;
#19629 = CARTESIAN_POINT ( 'NONE',  ( -2.077846259693550746, 39.65884927180063357, 94.16433879953098085 ) ) ;
#19630 = EDGE_LOOP ( 'NONE', ( #2498, #10177, #13996, #7300 ) ) ;
#19631 = CARTESIAN_POINT ( 'NONE',  ( 31.22215374030650281, 42.76218137147968434, 72.80433879953100984 ) ) ;
#19632 = DIRECTION ( 'NONE',  ( -1.402518428993830937E-16, 1.000000000000000000, -3.469446951953617147E-16 ) ) ;
#19633 = CARTESIAN_POINT ( 'NONE',  ( -4.176309363623030180, 42.45208065485131499, 93.42308879953097289 ) ) ;
#19634 = ORIENTED_EDGE ( 'NONE', *, *, #5900, .F. ) ;
#19635 =( NAMED_UNIT ( * ) SI_UNIT ( $, .STERADIAN. ) SOLID_ANGLE_UNIT ( ) );
#19636 = CARTESIAN_POINT ( 'NONE',  ( 11.22215374030649926, 42.76218137147968434, 80.55433879953099563 ) ) ;
#19637 = B_SPLINE_CURVE_WITH_KNOTS ( 'NONE', 3,
 ( #856, #8739, #15227, #20310, #20425, #12667, #21033, #12453, #10873, #16172 ),
 .UNSPECIFIED., .F., .F.,
 ( 4, 2, 2, 2, 4 ),
 ( 0.000000000000000000, 0.0001454262934834706935, 0.0002181394402252059860, 0.0002908525869669412785, 0.0005817051739339218052 ),
 .UNSPECIFIED. ) ;
#19638 = AXIS2_PLACEMENT_3D ( 'NONE', #2880, #4247, #7875 ) ;
#19639 = CARTESIAN_POINT ( 'NONE',  ( -4.537099264183358294, 37.70896829297682729, 76.38448585835440952 ) ) ;
#19640 = LINE ( 'NONE', #12956, #11985 ) ;
#19641 = EDGE_CURVE ( 'NONE', #8152, #14081, #12340, .T. ) ;
#19642 = CARTESIAN_POINT ( 'NONE',  ( 4.490969506678155199, 36.18237959297783135, 75.97723610431854979 ) ) ;
#19643 = ORIENTED_EDGE ( 'NONE', *, *, #4772, .T. ) ;
#19644 = CARTESIAN_POINT ( 'NONE',  ( -5.362109749382325319, 38.45089291097274753, 75.75643513208801494 ) ) ;
#19645 = CARTESIAN_POINT ( 'NONE',  ( 9.296966826988569466, 42.65732387124978686, 75.81656704941096336 ) ) ;
#19646 = EDGE_CURVE ( 'NONE', #16959, #18997, #5327, .T. ) ;
#19647 = DIRECTION ( 'NONE',  ( 1.110223024625156540E-16, 1.000000000000000000, 5.922860397471808077E-17 ) ) ;
#19648 = CARTESIAN_POINT ( 'NONE',  ( 1.606955356318995554, 52.89554470253639096, 79.36023959048891641 ) ) ;
#19649 = ORIENTED_EDGE ( 'NONE', *, *, #20989, .F. ) ;
#19650 = VECTOR ( 'NONE', #11845, 1000.000000000000000 ) ;
#19651 = EDGE_CURVE ( 'NONE', #13622, #15829, #1454, .T. ) ;
#19652 = ORIENTED_EDGE ( 'NONE', *, *, #16663, .F. ) ;
#19653 = FACE_OUTER_BOUND ( 'NONE', #19871, .T. ) ;
#19654 = ORIENTED_EDGE ( 'NONE', *, *, #20150, .T. ) ;
#19655 = CARTESIAN_POINT ( 'NONE',  ( -5.368445182934982185, 36.96218137147968008, 93.55433879953098142 ) ) ;
#19656 = CARTESIAN_POINT ( 'NONE',  ( 4.903891431458001549, 51.86598285117960216, 77.64500276804245971 ) ) ;
#19657 = CARTESIAN_POINT ( 'NONE',  ( 0.5981602388297567741, 52.96185312741366857, 75.36022115247205022 ) ) ;
#19658 = CARTESIAN_POINT ( 'NONE',  ( 4.149022253754741207, 51.51650688196784955, 78.63864101191019529 ) ) ;
#19659 = CARTESIAN_POINT ( 'NONE',  ( 0.7901638384306272078, 50.30062182352762079, 94.67308879782399345 ) ) ;
#19660 = CARTESIAN_POINT ( 'NONE',  ( -4.524181921268124462, 40.28999182795290324, 93.53933880123804556 ) ) ;
#19661 = CARTESIAN_POINT ( 'NONE',  ( 4.561823949912076515, 52.11865432047892455, 76.17419329630023128 ) ) ;
#19662 = CARTESIAN_POINT ( 'NONE',  ( -3.501354354950024117, 36.19377011966047775, 76.40804902690982203 ) ) ;
#19663 = CARTESIAN_POINT ( 'NONE',  ( -4.891140504938443989, 37.22034916465592147, 76.21310604893328389 ) ) ;
#19664 = VECTOR ( 'NONE', #11640, 1000.000000000000000 ) ;
#19665 = CARTESIAN_POINT ( 'NONE',  ( 5.611423337425062385, 41.22389019960463230, 91.42996380123798872 ) ) ;
#19666 = ORIENTED_EDGE ( 'NONE', *, *, #4537, .T. ) ;
#19667 = CARTESIAN_POINT ( 'NONE',  ( 6.282717385696039436, 38.32643750394947801, 78.79551527011911105 ) ) ;
#19668 = EDGE_LOOP ( 'NONE', ( #238, #16200, #525, #11297 ) ) ;
#19669 = CARTESIAN_POINT ( 'NONE',  ( 5.327803506469481754, 40.48109702276099853, 72.45433879953087342 ) ) ;
#19670 = EDGE_CURVE ( 'NONE', #5223, #16948, #15197, .T. ) ;
#19671 = CARTESIAN_POINT ( 'NONE',  ( -4.831226022076286597, 37.17609274966823563, 78.89646723195187406 ) ) ;
#19672 = FACE_OUTER_BOUND ( 'NONE', #14744, .T. ) ;
#19673 = CARTESIAN_POINT ( 'NONE',  ( 8.385738467910485383, 39.92631467184355643, 77.08252479744105301 ) ) ;
#19674 = ORIENTED_EDGE ( 'NONE', *, *, #19769, .T. ) ;
#19675 = EDGE_LOOP ( 'NONE', ( #16551, #10277, #13756, #1881, #14450, #7992, #13264, #15069, #4960, #2779, #13160, #4677 ) ) ;
#19676 = CIRCLE ( 'NONE', #4048, 8.199999999999995737 ) ;
#19677 = CARTESIAN_POINT ( 'NONE',  ( -0.1449331424556546677, 52.21320744800303260, 75.45826338387253429 ) ) ;
#19678 = LINE ( 'NONE', #1724, #16279 ) ;
#19679 = CARTESIAN_POINT ( 'NONE',  ( 7.751568289410731616, 40.29157170179672676, 78.99587745390167015 ) ) ;
#19680 = CARTESIAN_POINT ( 'NONE',  ( -7.677846259693480668, 36.96218137147968008, 95.05433879953098142 ) ) ;
#19681 = CARTESIAN_POINT ( 'NONE',  ( -4.159258199808826717, 37.42984277834096929, 78.62191134682883842 ) ) ;
#19682 = ORIENTED_EDGE ( 'NONE', *, *, #15640, .T. ) ;
#19683 = CARTESIAN_POINT ( 'NONE',  ( 8.371529501950854879, 41.80378517845067421, 76.20405737193274831 ) ) ;
#19684 = VECTOR ( 'NONE', #2427, 1000.000000000000000 ) ;
#19685 = VECTOR ( 'NONE', #12024, 1000.000000000000227 ) ;
#19686 = VERTEX_POINT ( 'NONE', #3386 ) ;
#19687 = CARTESIAN_POINT ( 'NONE',  ( 5.568489401881125289, 48.03437091500646261, 91.66433880123796030 ) ) ;
#19688 = CARTESIAN_POINT ( 'NONE',  ( -7.199730269989208509, 41.41414085053946081, 78.68823452940202401 ) ) ;
#19689 = CARTESIAN_POINT ( 'NONE',  ( -3.538351547904189154, 36.22109845575787546, 78.30834307773316993 ) ) ;
#19690 = EDGE_CURVE ( 'NONE', #15667, #7917, #11703, .T. ) ;
#19691 = CARTESIAN_POINT ( 'NONE',  ( 6.828503391016846891, 43.33193468930419101, 92.75808880123800293 ) ) ;
#19692 = CIRCLE ( 'NONE', #16656, 1.000000000000014655 ) ;
#19693 = AXIS2_PLACEMENT_3D ( 'NONE', #3660, #11665, #13250 ) ;
#19694 = DIRECTION ( 'NONE',  ( 3.893792155548169402E-16, 7.183611964723547524E-17, -1.000000000000000000 ) ) ;
#19695 = ORIENTED_EDGE ( 'NONE', *, *, #10403, .T. ) ;
#19696 = CARTESIAN_POINT ( 'NONE',  ( -0.8111795930268350663, 49.49551470481303284, 77.82100546619766135 ) ) ;
#19697 = ORIENTED_EDGE ( 'NONE', *, *, #17178, .T. ) ;
#19698 = VECTOR ( 'NONE', #18647, 1000.000000000000000 ) ;
#19699 = CARTESIAN_POINT ( 'NONE',  ( -7.607426330816210225, 47.53160628749161987, 78.30606788437694377 ) ) ;
#19700 = CARTESIAN_POINT ( 'NONE',  ( 6.198496396448986090, 45.68315280215533392, 90.49246380123798872 ) ) ;
#19701 = DIRECTION ( 'NONE',  ( -0.3165065846431827090, -0.9485903129789527988, 0.000000000000000000 ) ) ;
#19702 = ORIENTED_EDGE ( 'NONE', *, *, #10036, .F. ) ;
#19703 = CARTESIAN_POINT ( 'NONE',  ( -1.477846259693493813, 49.81903562097207327, 77.15433879953100416 ) ) ;
#19704 = CARTESIAN_POINT ( 'NONE',  ( 8.810541937945364666, 41.19947762056773399, 75.36738766396204880 ) ) ;
#19705 = CARTESIAN_POINT ( 'NONE',  ( 0.5221537403065015237, 44.16218137147968292, 75.45433879953088763 ) ) ;
#19706 = DIRECTION ( 'NONE',  ( 1.540237394707284220E-16, 1.793354297423764243E-16, -1.000000000000000000 ) ) ;
#19707 = CARTESIAN_POINT ( 'NONE',  ( -1.598719209087998694, 36.85794301744668644, 72.45433879953085921 ) ) ;
#19708 = ORIENTED_EDGE ( 'NONE', *, *, #15944, .F. ) ;
#19709 = CARTESIAN_POINT ( 'NONE',  ( -4.397525688316068937, 51.46253079027765409, 76.14127734336351239 ) ) ;
#19710 = EDGE_CURVE ( 'NONE', #16492, #2288, #16692, .T. ) ;
#19711 = B_SPLINE_CURVE_WITH_KNOTS ( 'NONE', 3,
 ( #8525, #527, #2455, #8734, #20201, #8842, #16715, #17027, #635, #11932, #5633, #13829, #13728, #3929 ),
 .UNSPECIFIED., .F., .F.,
 ( 4, 2, 2, 2, 2, 2, 4 ),
 ( 0.000000000000000000, 0.0003188956011945200857, 0.0004783434017918008368, 0.0006377912023890815879, 0.0007972390029863621764, 0.0009566868035836429817, 0.001275582404778193100 ),
 .UNSPECIFIED. ) ;
#19712 = ORIENTED_EDGE ( 'NONE', *, *, #5756, .F. ) ;
#19713 = LINE ( 'NONE', #1952, #9075 ) ;
#19714 = CARTESIAN_POINT ( 'NONE',  ( -6.782498427932185159, 40.54244403944807829, 77.72888818034803649 ) ) ;
#19715 = LINE ( 'NONE', #3749, #20699 ) ;
#19716 = CARTESIAN_POINT ( 'NONE',  ( 2.232254456934870124, 39.46371826755015633, 95.92308879611699979 ) ) ;
#19717 = COLOUR_RGB ( '', 0.09019608, 0.27058824, 0.51372549) ;
#19718 = CARTESIAN_POINT ( 'NONE',  ( -3.628867371436363509, 48.69222599884265179, 92.32933879782399345 ) ) ;
#19719 = CARTESIAN_POINT ( 'NONE',  ( 30.43948732994507722, 45.16218137147968292, 74.70433879953098710 ) ) ;
#19720 = APPLICATION_CONTEXT ( 'automotive_design' ) ;
#19721 = CARTESIAN_POINT ( 'NONE',  ( -7.001788291781583240, 47.28530462899436770, 78.29855163726114142 ) ) ;
#19722 = EDGE_CURVE ( 'NONE', #15570, #19783, #11909, .T. ) ;
#19723 = ORIENTED_EDGE ( 'NONE', *, *, #13413, .T. ) ;
#19724 = FACE_OUTER_BOUND ( 'NONE', #4492, .T. ) ;
#19725 = FACE_OUTER_BOUND ( 'NONE', #6695, .T. ) ;
#19726 = ORIENTED_EDGE ( 'NONE', *, *, #1731, .T. ) ;
#19727 = CARTESIAN_POINT ( 'NONE',  ( 2.263363662449363822, 49.77488197367694767, 93.11419268333823140 ) ) ;
#19728 = CARTESIAN_POINT ( 'NONE',  ( -0.4699484075730042676, 52.36218137147968577, 52.53721119516358584 ) ) ;
#19729 = CARTESIAN_POINT ( 'NONE',  ( 3.948530577815480225, 39.69684013992245752, 93.14871379953099506 ) ) ;
#19730 = EDGE_LOOP ( 'NONE', ( #10942, #12384, #5400, #2014, #12407, #4672, #2415 ) ) ;
#19731 = SURFACE_STYLE_USAGE ( .BOTH. , #3768 ) ;
#19732 = CARTESIAN_POINT ( 'NONE',  ( -4.387445420882217562, 37.78429639223235625, 75.36094808373545106 ) ) ;
#19733 = ORIENTED_EDGE ( 'NONE', *, *, #19641, .F. ) ;
#19734 = CARTESIAN_POINT ( 'NONE',  ( 0.3525650168280970997, 52.96056955190729099, 77.07067564994990505 ) ) ;
#19735 = CARTESIAN_POINT ( 'NONE',  ( -0.8237052942265477018, 49.18499566818285018, 94.94558879953099506 ) ) ;
#19736 = ORIENTED_EDGE ( 'NONE', *, *, #11832, .T. ) ;
#19737 = CARTESIAN_POINT ( 'NONE',  ( 8.887668352622405621, 41.43063037816333605, 75.36022115247205022 ) ) ;
#19738 = ORIENTED_EDGE ( 'NONE', *, *, #17953, .F. ) ;
#19739 = FACE_OUTER_BOUND ( 'NONE', #6421, .T. ) ;
#19740 = DIRECTION ( 'NONE',  ( -1.084202172485505420E-16, -1.000000000000000000, 0.000000000000000000 ) ) ;
#19741 = VECTOR ( 'NONE', #3943, 1000.000000000000000 ) ;
#19742 = CARTESIAN_POINT ( 'NONE',  ( 6.323093812904748923, 50.81767522096397727, 75.43719735689487038 ) ) ;
#19743 = CARTESIAN_POINT ( 'NONE',  ( 0.5789266213364873126, 51.36195753744342340, 77.38375056423674891 ) ) ;
#19744 = ADVANCED_FACE ( 'NONE', ( #10325 ), #193, .T. ) ;
#19745 = ORIENTED_EDGE ( 'NONE', *, *, #4787, .T. ) ;
#19746 = CARTESIAN_POINT ( 'NONE',  ( 3.990048841361577114, 36.74421560769709316, 76.25036098622081226 ) ) ;
#19747 = CARTESIAN_POINT ( 'NONE',  ( 8.387651578222229176, 39.93204838481331365, 78.28891658965622469 ) ) ;
#19748 = ORIENTED_EDGE ( 'NONE', *, *, #2595, .F. ) ;
#19749 = CIRCLE ( 'NONE', #19097, 1.399999999999995026 ) ;
#19750 = CARTESIAN_POINT ( 'NONE',  ( -0.9436870690626146807, 52.23009998296728895, 77.77566232894263010 ) ) ;
#19751 = CARTESIAN_POINT ( 'NONE',  ( -2.829262219629336883, 48.16467593588394891, 94.09494095006277803 ) ) ;
#19752 = DIRECTION ( 'NONE',  ( -0.2848220354341971516, 0.9585804129707224952, 1.280380753214897429E-16 ) ) ;
#19753 = CARTESIAN_POINT ( 'NONE',  ( -7.294472080575377326, 41.68420623513899415, 78.93669174070734584 ) ) ;
#19754 = AXIS2_PLACEMENT_3D ( 'NONE', #12964, #6460, #3075 ) ;
#19755 = ORIENTED_EDGE ( 'NONE', *, *, #9540, .T. ) ;
#19756 = DIRECTION ( 'NONE',  ( 1.290716872006552287E-16, 1.000000000000000000, 0.000000000000000000 ) ) ;
#19757 = VERTEX_POINT ( 'NONE', #10103 ) ;
#19758 = LINE ( 'NONE', #8708, #6038 ) ;
#19759 = EDGE_CURVE ( 'NONE', #6384, #20391, #6862, .T. ) ;
#19760 = CARTESIAN_POINT ( 'NONE',  ( 6.457023732898393931, 39.40536329938229443, 72.45433879953087342 ) ) ;
#19762 = EDGE_CURVE ( 'NONE', #13095, #10052, #19554, .T. ) ;
#19761 = SURFACE_STYLE_FILL_AREA ( #3186 ) ;
#19763 = DIRECTION ( 'NONE',  ( -1.402518428993831676E-16, 1.000000000000000000, -1.677918375355662166E-32 ) ) ;
#19764 = DIRECTION ( 'NONE',  ( 1.402518428993831676E-16, -1.000000000000000000, 0.000000000000000000 ) ) ;
#19765 = LINE ( 'NONE', #14669, #20840 ) ;
#19766 = CARTESIAN_POINT ( 'NONE',  ( -5.160557796315993428, 37.41935686500602287, 77.90139762306027649 ) ) ;
#19767 = FACE_OUTER_BOUND ( 'NONE', #6836, .T. ) ;
#19768 = CARTESIAN_POINT ( 'NONE',  ( 4.252148395930121616, 51.42256623072658073, 75.77039595153209461 ) ) ;
#19769 = EDGE_CURVE ( 'NONE', #12581, #6991, #2116, .T. ) ;
#19770 = CARTESIAN_POINT ( 'NONE',  ( 5.568489401881125289, 48.03437091500646261, 90.41433880123798872 ) ) ;
#19771 = VECTOR ( 'NONE', #7997, 1000.000000000000000 ) ;
#19772 = EDGE_CURVE ( 'NONE', #16377, #18140, #2215, .T. ) ;
#19773 = CARTESIAN_POINT ( 'NONE',  ( -5.154188915835984375, 42.64120994080404614, 90.96121380123797451 ) ) ;
#19774 = VERTEX_POINT ( 'NONE', #9902 ) ;
#19775 = CARTESIAN_POINT ( 'NONE',  ( 3.972684840124949268, 36.72331404565372281, 76.33233413694243552 ) ) ;
#19776 = DIRECTION ( 'NONE',  ( -0.6080936526121348829, -0.7938652969193402686, -2.360290325043241787E-16 ) ) ;
#19777 = CARTESIAN_POINT ( 'NONE',  ( 8.607847902093633152, 42.79549789786761949, 75.71644552919879345 ) ) ;
#19778 = VECTOR ( 'NONE', #4308, 1000.000000000000000 ) ;
#19779 = PLANE ( 'NONE',  #14623 ) ;
#19780 = DIRECTION ( 'NONE',  ( -0.3165065846431824870, -0.9485903129789529098, 0.000000000000000000 ) ) ;
#19781 = AXIS2_PLACEMENT_3D ( 'NONE', #12115, #13706, #10532 ) ;
#19782 = DIRECTION ( 'NONE',  ( 0.007885122365275663500, 0.9999689119394085113, 1.805443505845543142E-16 ) ) ;
#19783 = VERTEX_POINT ( 'NONE', #15097 ) ;
#19784 =( BOUNDED_CURVE ( )  B_SPLINE_CURVE ( 3, ( #9784, #12856, #11384, #14454 ),
 .UNSPECIFIED., .F., .F. ) 
 B_SPLINE_CURVE_WITH_KNOTS ( ( 4, 4 ),
 ( 4.188790204786389637, 4.300872134317200945 ),
 .UNSPECIFIED. ) 
 CURVE ( )  GEOMETRIC_REPRESENTATION_ITEM ( )  RATIONAL_B_SPLINE_CURVE ( ( 1.000000000000000000, 0.9989534107080366709, 0.9989534107080366709, 1.000000000000000000 ) ) 
 REPRESENTATION_ITEM ( '' )  );
#19785 = ORIENTED_EDGE ( 'NONE', *, *, #2841, .F. ) ;
#19786 = LINE ( 'NONE', #13, #11779 ) ;
#19787 = CARTESIAN_POINT ( 'NONE',  ( 0.5221537403065010796, 44.16218137147968292, 78.13669174070733447 ) ) ;
#19788 = CARTESIAN_POINT ( 'NONE',  ( 0.8495798803348756367, 52.95608793177016338, 76.37320741481380537 ) ) ;
#19789 = ORIENTED_EDGE ( 'NONE', *, *, #5484, .F. ) ;
#19790 = CARTESIAN_POINT ( 'NONE',  ( -4.393892947181490705, 51.46512661408927869, 78.70491066849456274 ) ) ;
#19791 = CARTESIAN_POINT ( 'NONE',  ( -4.518589064258794252, 36.94516042271330036, 78.67445481091525039 ) ) ;
#19792 = ORIENTED_EDGE ( 'NONE', *, *, #15109, .F. ) ;
#19793 = CARTESIAN_POINT ( 'NONE',  ( -2.077846259693550746, 39.65884927180063357, 94.47683880294496817 ) ) ;
#19794 = EDGE_CURVE ( 'NONE', #6337, #11401, #19029, .T. ) ;
#19795 = CARTESIAN_POINT ( 'NONE',  ( -7.794531540891230570, 41.26351018813655713, 78.81104446281315745 ) ) ;
#19796 = VECTOR ( 'NONE', #17801, 1000.000000000000000 ) ;
#19797 = CARTESIAN_POINT ( 'NONE',  ( -2.416137431568557314, 39.07291177436112406, 91.27371380123798872 ) ) ;
#19798 = CARTESIAN_POINT ( 'NONE',  ( 8.359199713419561917, 41.74790691855383784, 79.54611504273570688 ) ) ;
#19799 = ORIENTED_EDGE ( 'NONE', *, *, #18570, .T. ) ;
#19800 = DIRECTION ( 'NONE',  ( 0.000000000000000000, 0.000000000000000000, 1.000000000000000000 ) ) ;
#19801 = EDGE_LOOP ( 'NONE', ( #17436, #16029, #3198, #19921 ) ) ;
#19802 = CARTESIAN_POINT ( 'NONE',  ( -7.715124386663294587, 47.25851271173962687, 78.12178705274547497 ) ) ;
#19803 = B_SPLINE_CURVE_WITH_KNOTS ( 'NONE', 3,
 ( #214, #8527, #19988, #16822, #5415, #13205, #11934, #5535, #19681, #6915 ),
 .UNSPECIFIED., .F., .F.,
 ( 4, 2, 2, 2, 4 ),
 ( 0.000000000000000000, 0.0001226732940611538817, 0.0002453465881223077633, 0.0003680198821834616179, 0.0004906931762446155266 ),
 .UNSPECIFIED. ) ;
#19804 = CARTESIAN_POINT ( 'NONE',  ( 3.460444912181559474, 49.25145096859824889, 95.49246380123798872 ) ) ;
#19805 = ORIENTED_EDGE ( 'NONE', *, *, #6628, .F. ) ;
#19806 = DIRECTION ( 'NONE',  ( 0.9585804129707226062, 0.2848220354341972071, 1.987228219138359305E-16 ) ) ;
#19807 = FACE_OUTER_BOUND ( 'NONE', #3827, .T. ) ;
#19808 = AXIS2_PLACEMENT_3D ( 'NONE', #3933, #7559, #15336 ) ;
#19809 = CARTESIAN_POINT ( 'NONE',  ( 5.815517440877807864, 45.28237139676105016, 92.55433879953096721 ) ) ;
#19810 = DIRECTION ( 'NONE',  ( 0.007885122365275663500, 0.9999689119394085113, 1.805443505845543142E-16 ) ) ;
#19811 = CARTESIAN_POINT ( 'NONE',  ( 0.5221537403065048544, 39.16218137147969003, 93.66636871766883132 ) ) ;
#19812 = ORIENTED_EDGE ( 'NONE', *, *, #9778, .T. ) ;
#19813 = CARTESIAN_POINT ( 'NONE',  ( -4.537099264183358294, 37.70896829297682729, 72.45433879953085921 ) ) ;
#19814 = VERTEX_POINT ( 'NONE', #16586 ) ;
#19815 = CARTESIAN_POINT ( 'NONE',  ( -3.567022099613818664, 37.05453471803580356, 77.68963291717793140 ) ) ;
#19816 = CARTESIAN_POINT ( 'NONE',  ( -6.705728293473678825, 40.29967276483549199, 78.42124021397933120 ) ) ;
#19817 = LINE ( 'NONE', #14726, #13244 ) ;
#19818 = CARTESIAN_POINT ( 'NONE',  ( -3.134114116279071549, 48.15229756555780227, 91.62621379611699979 ) ) ;
#19819 = CARTESIAN_POINT ( 'NONE',  ( 0.2541436421823710656, 38.02374091943176637, 92.95433879782399345 ) ) ;
#19820 = CARTESIAN_POINT ( 'NONE',  ( 5.844285037446443454, 37.14940932322087264, 76.26708001093082601 ) ) ;
#19821 = VECTOR ( 'NONE', #1474, 1000.000000000000000 ) ;
#19822 = ORIENTED_EDGE ( 'NONE', *, *, #985, .T. ) ;
#19823 = CARTESIAN_POINT ( 'NONE',  ( 0.7119631482320658566, 52.96525702863522156, 79.54746358246200089 ) ) ;
#19824 = CARTESIAN_POINT ( 'NONE',  ( 0.5221537403065181771, 44.16218137147969003, 56.15433879953099705 ) ) ;
#19825 = EDGE_CURVE ( 'NONE', #17827, #6925, #405, .T. ) ;
#19826 = ORIENTED_EDGE ( 'NONE', *, *, #15206, .T. ) ;
#19827 = CARTESIAN_POINT ( 'NONE',  ( 0.5221537403065008576, 44.16218137147969003, 105.5543387995310098 ) ) ;
#19828 = FACE_BOUND ( 'NONE', #16688, .T. ) ;
#19829 = CARTESIAN_POINT ( 'NONE',  ( 3.948530577815480225, 39.69684013992245752, 94.39871379953098085 ) ) ;
#19830 = ORIENTED_EDGE ( 'NONE', *, *, #4239, .T. ) ;
#19831 = CARTESIAN_POINT ( 'NONE',  ( 8.911238338503892464, 41.50127112110217809, 78.09303657357962436 ) ) ;
#19832 = CARTESIAN_POINT ( 'NONE',  ( -5.508129029085064410, 38.61210022972240097, 76.73301527011911105 ) ) ;
#19833 = ORIENTED_EDGE ( 'NONE', *, *, #4035, .T. ) ;
#19834 = PLANE ( 'NONE',  #4680 ) ;
#19835 = LINE ( 'NONE', #3668, #17642 ) ;
#19836 = CARTESIAN_POINT ( 'NONE',  ( 5.025485839985549319, 41.56218137147963887, 91.97683879953100927 ) ) ;
#19837 = ORIENTED_EDGE ( 'NONE', *, *, #20369, .F. ) ;
#19838 = CARTESIAN_POINT ( 'NONE',  ( -4.383468690544193969, 37.62011356440623899, 77.91594000873737969 ) ) ;
#19839 = ORIENTED_EDGE ( 'NONE', *, *, #7931, .F. ) ;
#19840 = DIRECTION ( 'NONE',  ( 1.540237394707283727E-16, 1.793354297423763257E-16, -1.000000000000000000 ) ) ;
#19841 = DIRECTION ( 'NONE',  ( 1.000000000000000000, 0.000000000000000000, 0.000000000000000000 ) ) ;
#19842 = CARTESIAN_POINT ( 'NONE',  ( 5.521710135516018525, 50.48479211476082185, 75.36814786694185386 ) ) ;
#19843 =( BOUNDED_CURVE ( )  B_SPLINE_CURVE ( 2, ( #2759, #9360, #19329, #14131, #4747 ),
 .UNSPECIFIED., .F., .F. ) 
 B_SPLINE_CURVE_WITH_KNOTS ( ( 3, 2, 3 ),
 ( 0.4514241053481902743, 0.4687348658651156463, 0.4774649324440010667 ),
 .UNSPECIFIED. ) 
 CURVE ( )  GEOMETRIC_REPRESENTATION_ITEM ( )  RATIONAL_B_SPLINE_CURVE ( ( 0.9660722094251321668, 0.9493985640418991512, 1.000000000000000000, 0.9744809649195071977, 0.9660722070856953003 ) ) 
 REPRESENTATION_ITEM ( '' )  );
#19844 = CARTESIAN_POINT ( 'NONE',  ( 5.526420620081125001, 50.65814065400521571, 77.23783507897452694 ) ) ;
#19845 = CARTESIAN_POINT ( 'NONE',  ( 0.5221537403065019678, 44.16218137147968292, 72.45433879953087342 ) ) ;
#19846 = VERTEX_POINT ( 'NONE', #1810 ) ;
#19847 = ORIENTED_EDGE ( 'NONE', *, *, #19690, .T. ) ;
#19848 = EDGE_CURVE ( 'NONE', #4681, #5056, #9387, .T. ) ;
#19849 = CARTESIAN_POINT ( 'NONE',  ( 4.643940233704298315, 36.29168687389493897, 75.71841013695411959 ) ) ;
#19850 = CARTESIAN_POINT ( 'NONE',  ( 7.676056969765417293, 40.16377225106099758, 77.86095545630369941 ) ) ;
#19851 = ADVANCED_FACE ( 'NONE', ( #12219 ), #4011, .F. ) ;
#19852 = ORIENTED_EDGE ( 'NONE', *, *, #20704, .T. ) ;
#19853 = DIRECTION ( 'NONE',  ( 1.402518428993831676E-16, -1.000000000000000000, -0.000000000000000000 ) ) ;
#19854 = DIRECTION ( 'NONE',  ( -1.402518428993830937E-16, 1.000000000000000000, -3.469446951953617147E-16 ) ) ;
#19855 = CARTESIAN_POINT ( 'NONE',  ( -2.416137431568557314, 39.07291177436112406, 93.77371380123797451 ) ) ;
#19856 = ORIENTED_EDGE ( 'NONE', *, *, #15209, .T. ) ;
#19857 = ORIENTED_EDGE ( 'NONE', *, *, #19375, .T. ) ;
#19858 = DIRECTION ( 'NONE',  ( -1.540237394707284220E-16, -1.793354297423764243E-16, 1.000000000000000000 ) ) ;
#19859 = ORIENTED_EDGE ( 'NONE', *, *, #14631, .T. ) ;
#19860 = CARTESIAN_POINT ( 'NONE',  ( 2.522153740306506631, 50.16218137147969713, 77.55433879953099563 ) ) ;
#19861 = ADVANCED_FACE ( 'NONE', ( #7091 ), #20182, .F. ) ;
#19862 = CARTESIAN_POINT ( 'NONE',  ( 8.949781629519392823, 41.61678780941641520, 75.36311794487049553 ) ) ;
#19863 = CARTESIAN_POINT ( 'NONE',  ( -7.376208160937971492, 41.95857449956633900, 78.60633356588459719 ) ) ;
#19864 = DIRECTION ( 'NONE',  ( -0.5941461771851691553, -0.8043570849667760481, -2.357623395011396791E-16 ) ) ;
#19865 = CARTESIAN_POINT ( 'NONE',  ( 8.385679600361122255, 39.92613824206362949, 77.69330938776616335 ) ) ;
#19866 = CARTESIAN_POINT ( 'NONE',  ( 8.215888888258310985, 41.33732038555770316, 76.18655208513948196 ) ) ;
#19867 = ADVANCED_FACE ( 'NONE', ( #5508 ), #20282, .F. ) ;
#19868 = DIRECTION ( 'NONE',  ( -1.000000000000000000, 0.000000000000000000, 0.000000000000000000 ) ) ;
#19869 = CARTESIAN_POINT ( 'NONE',  ( 4.552447320970152589, 52.12558045856467004, 76.26690125110441443 ) ) ;
#19870 = CARTESIAN_POINT ( 'NONE',  ( 5.568489401881125289, 48.03437091500646261, 92.91433880123798872 ) ) ;
#19871 = EDGE_LOOP ( 'NONE', ( #20963, #10744, #8665, #1154 ) ) ;
#19872 = EDGE_CURVE ( 'NONE', #7261, #8801, #8927, .T. ) ;
#19873 = CARTESIAN_POINT ( 'NONE',  ( 0.3347249908012886466, 52.35620383029826286, 76.14768332476499779 ) ) ;
#19874 = ADVANCED_FACE ( 'NONE', ( #7420 ), #17323, .T. ) ;
#19875 = EDGE_CURVE ( 'NONE', #18535, #4997, #15416, .T. ) ;
#19876 = ORIENTED_EDGE ( 'NONE', *, *, #9988, .F. ) ;
#19877 = DIRECTION ( 'NONE',  ( -0.8660254037844351549, -1.050845190663206368E-16, 0.5000000000000061062 ) ) ;
#19878 = LINE ( 'NONE', #18399, #6167 ) ;
#19879 = CARTESIAN_POINT ( 'NONE',  ( -4.721994780338715003, 37.09540803149950960, 78.93613021445058564 ) ) ;
#19880 = CARTESIAN_POINT ( 'NONE',  ( 6.198496396448986090, 45.68315280215533392, 95.49246380123798872 ) ) ;
#19881 = PRODUCT_RELATED_PRODUCT_CATEGORY ( 'part', '', ( #10609 ) ) ;
#19882 = CARTESIAN_POINT ( 'NONE',  ( 8.947628219434415442, 41.61033390278195299, 77.32525259820312158 ) ) ;
#19883 = CYLINDRICAL_SURFACE ( 'NONE', #10304, 6.000000000000002665 ) ;
#19884 = EDGE_CURVE ( 'NONE', #9071, #4581, #5828, .T. ) ;
#19885 = LINE ( 'NONE', #18193, #2021 ) ;
#19886 = VERTEX_POINT ( 'NONE', #13593 ) ;
#19887 = CARTESIAN_POINT ( 'NONE',  ( 9.342575031381675998, 42.79401455314646086, 78.75800315165874110 ) ) ;
#19888 = CARTESIAN_POINT ( 'NONE',  ( 0.5221537403065020788, 52.36218137147968577, 87.21440135111343750 ) ) ;
#19889 = CARTESIAN_POINT ( 'NONE',  ( -0.02399531697664270338, 35.98038931794833672, 79.45433879953087342 ) ) ;
#19890 = ORIENTED_EDGE ( 'NONE', *, *, #19132, .T. ) ;
#19891 = CARTESIAN_POINT ( 'NONE',  ( -4.970565407269693203, 43.69858568107365926, 95.05433879953102405 ) ) ;
#19892 = CARTESIAN_POINT ( 'NONE',  ( -4.661432690376159371, 37.05067325523395283, 78.93441095796421791 ) ) ;
#19893 = CARTESIAN_POINT ( 'NONE',  ( 5.025485839985549319, 41.56218137147963887, 94.78933880294496817 ) ) ;
#19894 = CARTESIAN_POINT ( 'NONE',  ( 1.411666439545806506, 52.20714772099431400, 76.80858772049349170 ) ) ;
#19895 = CARTESIAN_POINT ( 'NONE',  ( -5.154188915835984375, 42.64120994080404614, 95.96121380123798872 ) ) ;
#19896 = PRODUCT ( 'Bushing', 'Bushing', '', ( #7295 ) ) ;
#19897 = CARTESIAN_POINT ( 'NONE',  ( -1.219056181836354558, 49.77488197367695477, 93.23425466814931895 ) ) ;
#19898 = ORIENTED_EDGE ( 'NONE', *, *, #12626, .F. ) ;
#19899 = EDGE_CURVE ( 'NONE', #20176, #12108, #11163, .T. ) ;
#19900 = DIRECTION ( 'NONE',  ( 0.000000000000000000, 1.000000000000000000, 1.734723475976787846E-14 ) ) ;
#19901 = ORIENTED_EDGE ( 'NONE', *, *, #16540, .F. ) ;
#19902 = DIRECTION ( 'NONE',  ( 0.007885122365275663500, 0.9999689119394085113, 1.805443505845543142E-16 ) ) ;
#19903 = EDGE_CURVE ( 'NONE', #12245, #8103, #17761, .T. ) ;
#19904 = CARTESIAN_POINT ( 'NONE',  ( -2.416137431568557314, 39.07291177436112406, 92.36746380123797451 ) ) ;
#19905 = ORIENTED_EDGE ( 'NONE', *, *, #603, .F. ) ;
#19906 = CARTESIAN_POINT ( 'NONE',  ( 6.924055141134583202, 50.37376929599953712, 78.48669174070734300 ) ) ;
#19907 = EDGE_CURVE ( 'NONE', #2983, #4618, #15627, .T. ) ;
#19908 = CARTESIAN_POINT ( 'NONE',  ( -1.219503646467430036, 49.90383875825363447, 69.41268141275705261 ) ) ;
#19909 = VECTOR ( 'NONE', #17470, 1000.000000000000000 ) ;
#19910 = DIRECTION ( 'NONE',  ( -1.540237394707284220E-16, -1.793354297423764243E-16, 1.000000000000000000 ) ) ;
#19911 = CARTESIAN_POINT ( 'NONE',  ( -1.590937568396969759, 39.63064243629642647, 93.57933879953097289 ) ) ;
#19912 = ORIENTED_EDGE ( 'NONE', *, *, #7854, .F. ) ;
#19913 = DIRECTION ( 'NONE',  ( -1.540237394707284220E-16, -1.793354297423764243E-16, 1.000000000000000000 ) ) ;
#19914 = VERTEX_POINT ( 'NONE', #17214 ) ;
#19915 = CARTESIAN_POINT ( 'NONE',  ( -3.130400440463537048, 36.82058224111691658, 78.12965606777083849 ) ) ;
#19916 = CARTESIAN_POINT ( 'NONE',  ( -6.960534101141536922, 41.10544874976162788, 76.96732277425439861 ) ) ;
#19917 = DIRECTION ( 'NONE',  ( 0.8236492988270800453, 0.5670994908670431434, 2.285625759191143542E-16 ) ) ;
#19918 = CARTESIAN_POINT ( 'NONE',  ( -7.507604988220667686, 45.82440120099734315, 75.45433879953087342 ) ) ;
#19919 = CARTESIAN_POINT ( 'NONE',  ( 6.660594192354429843, 43.89417127335556046, 93.26683879782399345 ) ) ;
#19920 = MECHANICAL_DESIGN_GEOMETRIC_PRESENTATION_REPRESENTATION (  '', ( #12472 ), #2957 ) ;
#19921 = ORIENTED_EDGE ( 'NONE', *, *, #6737, .T. ) ;
#19922 = CARTESIAN_POINT ( 'NONE',  ( 13.32277635493561974, 51.36218137147968577, 93.55433879953098142 ) ) ;
#19923 = CARTESIAN_POINT ( 'NONE',  ( 2.447781712115294273, 38.42313889284341144, 72.45433879953087342 ) ) ;
#19924 = VERTEX_POINT ( 'NONE', #15519 ) ;
#19925 = CARTESIAN_POINT ( 'NONE',  ( -1.477846259693498476, 49.81903562097206617, 67.21119304902336467 ) ) ;
#19926 = CARTESIAN_POINT ( 'NONE',  ( -0.2125050281363792815, 38.58189400963055959, 95.49246379953098085 ) ) ;
#19927 = CARTESIAN_POINT ( 'NONE',  ( 5.544968037009670780, 45.50804040601273925, 94.63308879953099506 ) ) ;
#19928 = CARTESIAN_POINT ( 'NONE',  ( -7.176159402432388923, 41.75141254259964541, 77.91116350996777840 ) ) ;
#19929 = ORIENTED_EDGE ( 'NONE', *, *, #2624, .T. ) ;
#19930 = DIRECTION ( 'NONE',  ( -0.5800177190770223756, -0.8146038580541392626, -2.354238310054622287E-16 ) ) ;
#19931 = CARTESIAN_POINT ( 'NONE',  ( -5.954976305145402549, 38.00616181634879354, 76.59693911441793546 ) ) ;
#19932 = ORIENTED_EDGE ( 'NONE', *, *, #1286, .F. ) ;
#19933 = LINE ( 'NONE', #13461, #11844 ) ;
#19934 = CARTESIAN_POINT ( 'NONE',  ( 0.3849501894475816366, 52.96112454960368865, 76.04253343019715317 ) ) ;
#19935 = VERTEX_POINT ( 'NONE', #2639 ) ;
#19936 = LINE ( 'NONE', #3360, #19032 ) ;
#19937 =( GEOMETRIC_REPRESENTATION_CONTEXT ( 3 ) GLOBAL_UNCERTAINTY_ASSIGNED_CONTEXT ( ( #7021 ) ) GLOBAL_UNIT_ASSIGNED_CONTEXT ( ( #16252, #9565, #19635 ) ) REPRESENTATION_CONTEXT ( 'NONE', 'WORKASPACE' ) );
#19938 = ORIENTED_EDGE ( 'NONE', *, *, #19611, .T. ) ;
#19939 = CARTESIAN_POINT ( 'NONE',  ( -4.296394040159018601, 50.78788033116449441, 75.97399450257033493 ) ) ;
#19940 = CARTESIAN_POINT ( 'NONE',  ( 3.544512597232735818, 48.49373303889355213, 93.87251462254160117 ) ) ;
#19941 = LINE ( 'NONE', #2195, #4409 ) ;
#19942 = VECTOR ( 'NONE', #18101, 1000.000000000000000 ) ;
#19943 = LINE ( 'NONE', #19743, #2467 ) ;
#19944 = ORIENTED_EDGE ( 'NONE', *, *, #6328, .F. ) ;
#19945 = EDGE_LOOP ( 'NONE', ( #19180, #7972, #18771, #15319 ) ) ;
#19946 = CARTESIAN_POINT ( 'NONE',  ( 3.959708321255010599, 36.72253538286627617, 76.60595702694484999 ) ) ;
#19947 = AXIS2_PLACEMENT_3D ( 'NONE', #20598, #15620, #7414 ) ;
#19948 = EDGE_LOOP ( 'NONE', ( #2504, #10573, #5966, #13857 ) ) ;
#19949 = LINE ( 'NONE', #2201, #1348 ) ;
#19950 = LINE ( 'NONE', #1894, #16745 ) ;
#19951 = CARTESIAN_POINT ( 'NONE',  ( 5.568489401881125289, 48.03437091500646261, 95.57058880123798872 ) ) ;
#19952 = ORIENTED_EDGE ( 'NONE', *, *, #8307, .T. ) ;
#19953 = DIRECTION ( 'NONE',  ( -0.000000000000000000, -0.000000000000000000, 1.000000000000000000 ) ) ;
#19954 = VERTEX_POINT ( 'NONE', #7534 ) ;
#19955 = CARTESIAN_POINT ( 'NONE',  ( -3.936408902674054300, 36.51512738899805299, 77.68304435440727218 ) ) ;
#19956 = CARTESIAN_POINT ( 'NONE',  ( 7.906618077272564271, 40.87154522579304938, 75.47105533938442079 ) ) ;
#19957 = VECTOR ( 'NONE', #16038, 1000.000000000000000 ) ;
#19958 = CARTESIAN_POINT ( 'NONE',  ( 4.658006975973914443, 39.57252462080383992, 92.61876351041205169 ) ) ;
#19959 = FACE_OUTER_BOUND ( 'NONE', #16890, .T. ) ;
#19960 = CARTESIAN_POINT ( 'NONE',  ( -5.510796958474739604, 38.60848837797752964, 72.45433879953085921 ) ) ;
#19961 = EDGE_CURVE ( 'NONE', #4927, #15997, #20506, .T. ) ;
#19962 = CARTESIAN_POINT ( 'NONE',  ( -0.9988176903691428077, 49.83852402762217082, 95.80496380123798872 ) ) ;
#19963 = CARTESIAN_POINT ( 'NONE',  ( 8.212437538920868363, 41.32697647264386376, 76.28640183395299346 ) ) ;
#19964 = CARTESIAN_POINT ( 'NONE',  ( 6.919062940419317798, 50.37745683356979498, 76.08942471621537607 ) ) ;
#19966 = CARTESIAN_POINT ( 'NONE',  ( 5.902048492000326441, 51.12868443877599134, 78.59183879953087626 ) ) ;
#19965 = B_SPLINE_CURVE_WITH_KNOTS ( 'NONE', 3,
 ( #2480, #11571, #20007, #7036, #20220, #8871, #3851, #7471, #15458, #10372, #12162, #5558, #18756, #5655 ),
 .UNSPECIFIED., .F., .F.,
 ( 4, 2, 2, 2, 2, 2, 4 ),
 ( 4.336808689942017736E-19, 6.529564833732798800E-05, 0.0001305912966746555423, 0.0001958869450119831237, 0.0002611825933493106509, 0.0003917738900239288967, 0.0005223651866985471424 ),
 .UNSPECIFIED. ) ;
#19967 = CARTESIAN_POINT ( 'NONE',  ( 5.722153740306477054, 44.16218185475116798, 93.64411094854726514 ) ) ;
#19968 = CARTESIAN_POINT ( 'NONE',  ( 2.043125170982144745, 38.48583871533720213, 91.27371380123798872 ) ) ;
#19969 = DIRECTION ( 'NONE',  ( -1.621236893436268647E-16, -2.273814620809075225E-32, 1.000000000000000000 ) ) ;
#19970 = ORIENTED_EDGE ( 'NONE', *, *, #863, .T. ) ;
#19971 = CARTESIAN_POINT ( 'NONE',  ( 0.3395453217024830272, 52.96750455883004349, 76.14768332476499779 ) ) ;
#19972 = AXIS2_PLACEMENT_3D ( 'NONE', #18653, #20343, #2493 ) ;
#19973 = ORIENTED_EDGE ( 'NONE', *, *, #18361, .F. ) ;
#19974 = CARTESIAN_POINT ( 'NONE',  ( 0.5221537403065077410, 44.16218137147969713, 66.55433879953099563 ) ) ;
#19975 = EDGE_CURVE ( 'NONE', #271, #9577, #7615, .T. ) ;
#19976 = DIRECTION ( 'NONE',  ( -1.000000000000000000, 1.110223024625156540E-16, -1.779391786395883043E-16 ) ) ;
#19977 = CARTESIAN_POINT ( 'NONE',  ( 5.385333739904544004, 50.76442899832089495, 78.93605272602964362 ) ) ;
#19978 = CARTESIAN_POINT ( 'NONE',  ( -4.567115856812060670, 47.10047254335474065, 92.21121380123797451 ) ) ;
#19979 = CARTESIAN_POINT ( 'NONE',  ( 6.691294758883309157, 37.75465145915448062, 78.79551527011911105 ) ) ;
#19980 = CARTESIAN_POINT ( 'NONE',  ( 0.5221537403065006355, 48.36218137147969287, 92.45433879953097289 ) ) ;
#19981 = ADVANCED_BREP_SHAPE_REPRESENTATION ( '', ( #11462, #18366 ), #17679 ) ;
#19982 = EDGE_CURVE ( 'NONE', #9317, #12054, #12952, .T. ) ;
#19983 = CARTESIAN_POINT ( 'NONE',  ( 1.868012774839550749, 39.13936707477651566, 93.38308880294498238 ) ) ;
#19984 = ORIENTED_EDGE ( 'NONE', *, *, #13645, .T. ) ;
#19985 = ORIENTED_EDGE ( 'NONE', *, *, #12362, .T. ) ;
#19986 = CARTESIAN_POINT ( 'NONE',  ( 9.026706097321888222, 41.84733531941775198, 79.51559944055343010 ) ) ;
#19987 = CARTESIAN_POINT ( 'NONE',  ( 4.722153740306518799, 44.16218137147969003, 56.15433879953099705 ) ) ;
#19988 = CARTESIAN_POINT ( 'NONE',  ( -4.281535647588993854, 37.51643706874827444, 78.93136397943298732 ) ) ;
#19989 = VERTEX_POINT ( 'NONE', #15941 ) ;
#19990 = LINE ( 'NONE', #9951, #11330 ) ;
#19991 = CARTESIAN_POINT ( 'NONE',  ( -3.226449543290803135, 47.76606447477306716, 95.05433879953076826 ) ) ;
#19992 = CARTESIAN_POINT ( 'NONE',  ( 1.256812508749381774, 49.74246873332880625, 90.17996380294496817 ) ) ;
#19993 = CARTESIAN_POINT ( 'NONE',  ( 1.764424261053175957, 52.20436609593109267, 76.95808337915808295 ) ) ;
#19994 = CARTESIAN_POINT ( 'NONE',  ( -0.3080929418689875576, 37.85583172076933778, 93.69558880123800293 ) ) ;
#19995 = CARTESIAN_POINT ( 'NONE',  ( 5.497743849324330689, 37.64424434608246628, 72.45433879953087342 ) ) ;
#19996 = ORIENTED_EDGE ( 'NONE', *, *, #12369, .T. ) ;
#19997 = DIRECTION ( 'NONE',  ( -0.3165065846431827645, -0.9485903129789529098, 0.000000000000000000 ) ) ;
#19998 = VECTOR ( 'NONE', #13023, 1000.000000000000000 ) ;
#19999 = ORIENTED_EDGE ( 'NONE', *, *, #15762, .F. ) ;
#20000 = CARTESIAN_POINT ( 'NONE',  ( 31.07218010054375412, 42.96218137147968008, 65.80574467885102763 ) ) ;
#20001 = CARTESIAN_POINT ( 'NONE',  ( -5.784195910403845176, 44.99242805365518194, 92.13308880123798872 ) ) ;
#20002 = ORIENTED_EDGE ( 'NONE', *, *, #16864, .T. ) ;
#20003 = CARTESIAN_POINT ( 'NONE',  ( 8.364834758477957877, 41.76689748495397936, 78.11247371284943597 ) ) ;
#20005 = CIRCLE ( 'NONE', #5750, 3.200000000000009504 ) ;
#20004 = CARTESIAN_POINT ( 'NONE',  ( 0.5221537403065009686, 44.16218137147968292, 79.40903933791013003 ) ) ;
#20006 = CARTESIAN_POINT ( 'NONE',  ( -4.036263108762779162, 50.80090022068082334, 79.54642512701808243 ) ) ;
#20007 = CARTESIAN_POINT ( 'NONE',  ( 0.6354033039974273933, 52.96147787572222398, 77.38615267430542133 ) ) ;
#20008 = CARTESIAN_POINT ( 'NONE',  ( 5.379053567747686060, 50.76036377979792746, 77.28905211432859801 ) ) ;
#20009 = CARTESIAN_POINT ( 'NONE',  ( -0.4699484075730042676, 52.36218137147968577, 48.36106904222365444 ) ) ;
#20010 = VERTEX_POINT ( 'NONE', #7853 ) ;
#20011 = EDGE_CURVE ( 'NONE', #10514, #17974, #4851, .T. ) ;
#20012 = CARTESIAN_POINT ( 'NONE',  ( 5.391786323697940198, 50.75965653268888644, 77.94845644658968808 ) ) ;
#20013 = VECTOR ( 'NONE', #8132, 1000.000000000000000 ) ;
#20014 = ORIENTED_EDGE ( 'NONE', *, *, #9120, .F. ) ;
#20015 = DIRECTION ( 'NONE',  ( 1.540237394707284220E-16, 1.793354297423764243E-16, -1.000000000000000000 ) ) ;
#20016 = EDGE_CURVE ( 'NONE', #4192, #1854, #7642, .T. ) ;
#20017 = CARTESIAN_POINT ( 'NONE',  ( 31.22215374030650281, 42.76218137147968434, 77.40433879953098995 ) ) ;
#20018 = CIRCLE ( 'NONE', #20690, 8.199999999999995737 ) ;
#20019 = CARTESIAN_POINT ( 'NONE',  ( -7.880212061628153464, 41.54679441531448703, 76.16022115247204738 ) ) ;
#20020 = DIRECTION ( 'NONE',  ( -0.5941461771851692664, -0.8043570849667761591, -2.357623395011396791E-16 ) ) ;
#20021 = CARTESIAN_POINT ( 'NONE',  ( 0.7901638384306272078, 50.30062182352762079, 94.67308879782399345 ) ) ;
#20022 = B_SPLINE_CURVE_WITH_KNOTS ( 'NONE', 3,
 ( #9355, #20703, #20814, #15840, #7744, #6143, #11267, #14226, #12645, #19127, #16152, #6242, #21011, #12745, #6445, #19221, #5059, #3575 ),
 .UNSPECIFIED., .F., .F.,
 ( 4, 2, 2, 2, 2, 2, 2, 2, 4 ),
 ( 0.000000000000000000, 0.0002949345114877292926, 0.0005898690229754585852, 0.0008848035344631878778, 0.001179738045950917170, 0.001474672557438646463, 0.001769607068926375756, 0.002064541580414105265, 0.002359476091901834341 ),
 .UNSPECIFIED. ) ;
#20023 = CARTESIAN_POINT ( 'NONE',  ( 5.493332137868558007, 37.64554666260850979, 76.40678776405631822 ) ) ;
#20024 = ADVANCED_FACE ( 'NONE', ( #7955 ), #17529, .F. ) ;
#20025 = EDGE_CURVE ( 'NONE', #3298, #9436, #15737, .T. ) ;
#20026 = VECTOR ( 'NONE', #9108, 1000.000000000000000 ) ;
#20027 = VECTOR ( 'NONE', #1334, 1000.000000000000227 ) ;
#20028 = ORIENTED_EDGE ( 'NONE', *, *, #412, .F. ) ;
#20029 = CARTESIAN_POINT ( 'NONE',  ( 8.814092166714758037, 41.21011788141189669, 78.88950904781501094 ) ) ;
#20030 = ORIENTED_EDGE ( 'NONE', *, *, #16600, .F. ) ;
#20031 = CARTESIAN_POINT ( 'NONE',  ( 2.522153740306507075, 50.16218137147969713, 75.55433879953099563 ) ) ;
#20032 = CARTESIAN_POINT ( 'NONE',  ( -0.2125050281363792815, 38.58189400963055959, 94.24246379953099506 ) ) ;
#20033 = CARTESIAN_POINT ( 'NONE',  ( 3.122153740306552905, 48.66551347115873227, 93.53933879953099506 ) ) ;
#20034 = CIRCLE ( 'NONE', #16323, 8.199999999999995737 ) ;
#20035 = CARTESIAN_POINT ( 'NONE',  ( -7.913096914557509187, 41.63124252803902436, 77.76017221056694950 ) ) ;
#20036 = VERTEX_POINT ( 'NONE', #6033 ) ;
#20037 = VECTOR ( 'NONE', #16548, 1000.000000000000114 ) ;
#20038 = CARTESIAN_POINT ( 'NONE',  ( 9.012782495821852535, 41.80560540242532852, 78.13577067582016866 ) ) ;
#20039 = CYLINDRICAL_SURFACE ( 'NONE', #6537, 8.199999999999995737 ) ;
#20040 = ORIENTED_EDGE ( 'NONE', *, *, #3917, .T. ) ;
#20041 = CARTESIAN_POINT ( 'NONE',  ( 0.5819204035424812016, 38.92295143466739660, 95.05433879953096721 ) ) ;
#20042 = DIRECTION ( 'NONE',  ( -1.540237394707284467E-16, -1.793354297423764243E-16, 1.000000000000000000 ) ) ;
#20043 = ORIENTED_EDGE ( 'NONE', *, *, #15630, .F. ) ;
#20044 = LINE ( 'NONE', #904, #2385 ) ;
#20045 = CARTESIAN_POINT ( 'NONE',  ( -4.524181921268124462, 40.28999182795290324, 93.69558880123800293 ) ) ;
#20046 = VECTOR ( 'NONE', #12877, 1000.000000000000000 ) ;
#20047 = ORIENTED_EDGE ( 'NONE', *, *, #17856, .T. ) ;
#20048 = CARTESIAN_POINT ( 'NONE',  ( 0.8455950101471348956, 52.35579997042385259, 77.76169174070734869 ) ) ;
#20049 = CARTESIAN_POINT ( 'NONE',  ( 5.327803506469481754, 40.48109702276099853, 72.45432679953087529 ) ) ;
#20050 = CARTESIAN_POINT ( 'NONE',  ( -5.154188915835984375, 42.64120994080404614, 90.96121380123797451 ) ) ;
#20051 = SHAPE_DEFINITION_REPRESENTATION ( #16862, #333 ) ;
#20052 = DIRECTION ( 'NONE',  ( -0.9485903129789527988, 0.3165065846431829311, -8.934458285744989980E-17 ) ) ;
#20053 = ADVANCED_FACE ( 'NONE', ( #4542 ), #12533, .T. ) ;
#20054 = VECTOR ( 'NONE', #3392, 1000.000000000000227 ) ;
#20055 = CARTESIAN_POINT ( 'NONE',  ( 4.512269934384612213, 47.81844922806527620, 94.12621379953098710 ) ) ;
#20056 = CARTESIAN_POINT ( 'NONE',  ( -3.411370229937075393, 36.96692943841399881, 79.28278856980307410 ) ) ;
#20057 = EDGE_LOOP ( 'NONE', ( #17386, #2002, #15066, #3220 ) ) ;
#20058 = EDGE_LOOP ( 'NONE', ( #255, #17928, #8023, #7608 ) ) ;
#20059 = CARTESIAN_POINT ( 'NONE',  ( 1.708921718063434181, 52.95755783200097966, 75.60954117182248524 ) ) ;
#20060 = ORIENTED_EDGE ( 'NONE', *, *, #13883, .T. ) ;
#20061 = CARTESIAN_POINT ( 'NONE',  ( -0.9098995361875932275, 52.23616864758587042, 78.71676077850084141 ) ) ;
#20062 = CARTESIAN_POINT ( 'NONE',  ( 0.3451640418029088275, 52.96747521092283506, 77.57937361552639288 ) ) ;
#20063 = CARTESIAN_POINT ( 'NONE',  ( -7.232783645916265769, 41.49729498405194761, 78.88165857690459859 ) ) ;
#20064 = CARTESIAN_POINT ( 'NONE',  ( -3.349688636638950889, 52.21127678364309332, 76.69845644658968808 ) ) ;
#20065 = EDGE_LOOP ( 'NONE', ( #6882, #13069, #10224, #18085 ) ) ;
#20066 = VERTEX_POINT ( 'NONE', #4441 ) ;
#20067 = DIRECTION ( 'NONE',  ( 0.007885122365275663500, 0.9999689119394085113, 1.805443505845543142E-16 ) ) ;
#20068 = EDGE_LOOP ( 'NONE', ( #14687, #13321, #2099, #13497 ) ) ;
#20069 = CARTESIAN_POINT ( 'NONE',  ( -3.537323694296532040, 36.22033922170236764, 77.24173421363296654 ) ) ;
#20070 = LINE ( 'NONE', #16998, #18322 ) ;
#20071 = FACE_OUTER_BOUND ( 'NONE', #19338, .T. ) ;
#20072 = FACE_OUTER_BOUND ( 'NONE', #8353, .T. ) ;
#20073 = CARTESIAN_POINT ( 'NONE',  ( -7.568569179903653854, 42.82598212476965216, 79.20830338942023729 ) ) ;
#20074 = CARTESIAN_POINT ( 'NONE',  ( -0.3080929418689875576, 37.85583172076933778, 95.10183880123796030 ) ) ;
#20075 = PRODUCT_DEFINITION_SHAPE ( 'NONE', 'NONE',  #11075 ) ;
#20076 = CARTESIAN_POINT ( 'NONE',  ( 8.787829143201870252, 41.13140593384865440, 76.40801527011910821 ) ) ;
#20077 = CARTESIAN_POINT ( 'NONE',  ( 23.03948732994508575, 43.16218137147969003, 76.90433879953101837 ) ) ;
#20078 = CARTESIAN_POINT ( 'NONE',  ( -4.211488180634966660, 48.16625856408043660, 78.25433879953088478 ) ) ;
#20079 = CARTESIAN_POINT ( 'NONE',  ( 3.460444912181559474, 49.25145096859824889, 94.24246380123798872 ) ) ;
#20080 = LINE ( 'NONE', #9819, #5851 ) ;
#20081 = CARTESIAN_POINT ( 'NONE',  ( 0.3318037965577209092, 52.35622686498843592, 76.19791476666895846 ) ) ;
#20082 = VECTOR ( 'NONE', #12033, 1000.000000000000000 ) ;
#20083 = EDGE_LOOP ( 'NONE', ( #9971, #17355, #7936, #8460 ) ) ;
#20084 = CARTESIAN_POINT ( 'NONE',  ( -3.567022099613818664, 37.05453471803580356, 77.68963291717793140 ) ) ;
#20085 = DIRECTION ( 'NONE',  ( 1.193617070626243484E-16, 1.000000000000000000, 0.000000000000000000 ) ) ;
#20086 = CARTESIAN_POINT ( 'NONE',  ( -3.553498346352079285, 52.06564182703182553, 79.13154374754441278 ) ) ;
#20087 = CARTESIAN_POINT ( 'NONE',  ( -0.9988176903691428077, 49.83852402762217082, 94.55496380123798872 ) ) ;
#20088 = ADVANCED_FACE ( 'NONE', ( #1252 ), #1363, .F. ) ;
#20089 = LINE ( 'NONE', #8727, #18711 ) ;
#20090 = DIRECTION ( 'NONE',  ( -1.000000000000000000, -1.621236893436269386E-16, 0.000000000000000000 ) ) ;
#20091 = CARTESIAN_POINT ( 'NONE',  ( 11.22215374030650281, 42.76218137147968434, 56.80715055817104542 ) ) ;
#20092 = CARTESIAN_POINT ( 'NONE',  ( 5.900862589321786977, 51.12956041731354873, 78.19629421043239859 ) ) ;
#20093 = ORIENTED_EDGE ( 'NONE', *, *, #2211, .T. ) ;
#20094 = VECTOR ( 'NONE', #230, 1000.000000000000000 ) ;
#20095 = CARTESIAN_POINT ( 'NONE',  ( 8.203713612165559610, 41.74519268224744906, 79.54698768757486960 ) ) ;
#20096 = CARTESIAN_POINT ( 'NONE',  ( -1.483269432489140449, 51.49895708687498086, 75.45433879953087342 ) ) ;
#20097 = CARTESIAN_POINT ( 'NONE',  ( 0.8478793724089639383, 52.95615112447037376, 76.25678054482114021 ) ) ;
#20098 = ORIENTED_EDGE ( 'NONE', *, *, #12464, .T. ) ;
#20099 = LINE ( 'NONE', #12143, #14381 ) ;
#20100 = DIRECTION ( 'NONE',  ( -0.000000000000000000, -0.000000000000000000, 1.000000000000000000 ) ) ;
#20101 = ADVANCED_FACE ( 'NONE', ( #4738 ), #2852, .F. ) ;
#20102 = CARTESIAN_POINT ( 'NONE',  ( -4.621383371311750921, 37.02109043652605180, 78.92211507803222048 ) ) ;
#20103 = CARTESIAN_POINT ( 'NONE',  ( 1.868012774839550749, 39.13936707477651566, 90.88308880294496817 ) ) ;
#20104 = CARTESIAN_POINT ( 'NONE',  ( -7.279083289042354465, 41.66508001738827005, 78.93576421268289778 ) ) ;
#20105 = CARTESIAN_POINT ( 'NONE',  ( -7.722494531574873200, 47.25182341447533929, 78.06303731277932911 ) ) ;
#20106 = CARTESIAN_POINT ( 'NONE',  ( 3.122075258343615545, 38.59543968120053847, 90.21201841395856036 ) ) ;
#20107 = VECTOR ( 'NONE', #1134, 1000.000000000000000 ) ;
#20108 = CARTESIAN_POINT ( 'NONE',  ( 6.859321636172213132, 37.87471731380851026, 76.18799845131768222 ) ) ;
#20109 = EDGE_LOOP ( 'NONE', ( #4315, #16208, #11335, #20828 ) ) ;
#20110 = VECTOR ( 'NONE', #6383, 1000.000000000000000 ) ;
#20111 = CARTESIAN_POINT ( 'NONE',  ( 5.563695719829709674, 50.62397605989450255, 77.13671500005938242 ) ) ;
#20112 = ORIENTED_EDGE ( 'NONE', *, *, #19482, .F. ) ;
#20113 = EDGE_CURVE ( 'NONE', #14094, #16863, #20022, .T. ) ;
#20114 = CARTESIAN_POINT ( 'NONE',  ( -4.451010579348070095, 50.67739701313279710, 78.52518475144754007 ) ) ;
#20115 = CARTESIAN_POINT ( 'NONE',  ( -4.524181921268124462, 40.28999182795290324, 93.53933880123797451 ) ) ;
#20116 = ORIENTED_EDGE ( 'NONE', *, *, #5746, .T. ) ;
#20117 = CARTESIAN_POINT ( 'NONE',  ( 2.522153740306511072, 47.62628298661745418, 50.55433879953100273 ) ) ;
#20118 = DIRECTION ( 'NONE',  ( 0.000000000000000000, 0.000000000000000000, 1.000000000000000000 ) ) ;
#20119 = CARTESIAN_POINT ( 'NONE',  ( -3.935607453025473657, 50.87282506703193974, 79.53937015691786883 ) ) ;
#20120 = FACE_OUTER_BOUND ( 'NONE', #5500, .T. ) ;
#20121 = CARTESIAN_POINT ( 'NONE',  ( 5.760694563098077481, 51.23309689197249384, 79.54845644658969661 ) ) ;
#20122 = CARTESIAN_POINT ( 'NONE',  ( 0.5221537403065188432, 44.16218137147969003, 54.55433879953099563 ) ) ;
#20123 = ORIENTED_EDGE ( 'NONE', *, *, #11071, .T. ) ;
#20124 = DIRECTION ( 'NONE',  ( -1.540237394707284220E-16, -1.793354297423764243E-16, 1.000000000000000000 ) ) ;
#20125 = VECTOR ( 'NONE', #20600, 1000.000000000000000 ) ;
#20126 = ADVANCED_FACE ( 'NONE', ( #10080 ), #1676, .T. ) ;
#20127 = EDGE_LOOP ( 'NONE', ( #5930, #11749, #13060, #6903 ) ) ;
#20128 = LINE ( 'NONE', #8767, #10109 ) ;
#20129 = CARTESIAN_POINT ( 'NONE',  ( 6.961907239250668233, 50.34580947589670075, 76.63889762306028786 ) ) ;
#20130 = CARTESIAN_POINT ( 'NONE',  ( 5.491862665586171310, 37.63975666314849633, 76.14240822758154081 ) ) ;
#20131 = EDGE_CURVE ( 'NONE', #2164, #8338, #11578, .T. ) ;
#20132 = CARTESIAN_POINT ( 'NONE',  ( -5.529385682154831727, 44.31555110708731604, 72.45432679953087529 ) ) ;
#20133 = CARTESIAN_POINT ( 'NONE',  ( -5.616286711741430793, 44.43019146960381960, 93.89183879782397923 ) ) ;
#20134 = CARTESIAN_POINT ( 'NONE',  ( -5.868264228364990842, 37.94211109820661676, 75.91870325888974946 ) ) ;
#20135 = EDGE_LOOP ( 'NONE', ( #10310, #2593, #11723, #5680, #17809, #14564 ) ) ;
#20136 = CARTESIAN_POINT ( 'NONE',  ( 8.789256573544019346, 41.13568403313856692, 78.71078388337100762 ) ) ;
#20137 = EDGE_CURVE ( 'NONE', #11865, #8000, #13468, .T. ) ;
#20138 = VERTEX_POINT ( 'NONE', #3475 ) ;
#20139 = VECTOR ( 'NONE', #12635, 1000.000000000000000 ) ;
#20140 = CARTESIAN_POINT ( 'NONE',  ( -4.230491984614289436, 51.58188695944873103, 75.39163409230444302 ) ) ;
#20141 = EDGE_CURVE ( 'NONE', #6705, #1396, #8160, .T. ) ;
#20142 = CARTESIAN_POINT ( 'NONE',  ( -5.058133621542618030, 44.89684013992257405, 95.17996379953099506 ) ) ;
#20143 = CARTESIAN_POINT ( 'NONE',  ( -2.904223097202481174, 48.62752260303690122, 92.52371379953099506 ) ) ;
#20144 = ORIENTED_EDGE ( 'NONE', *, *, #9105, .F. ) ;
#20145 = CARTESIAN_POINT ( 'NONE',  ( -0.9988176903691428077, 49.83852402762217082, 94.55496380123798872 ) ) ;
#20146 = CARTESIAN_POINT ( 'NONE',  ( 0.3529277580979759410, 52.96057327895140077, 77.54150982395135827 ) ) ;
#20147 = EDGE_LOOP ( 'NONE', ( #15832, #12631, #7056, #4046, #1849, #284, #11587 ) ) ;
#20148 = CARTESIAN_POINT ( 'NONE',  ( -4.746143138089100155, 42.07168972858362821, 95.05433879953095300 ) ) ;
#20149 = FACE_OUTER_BOUND ( 'NONE', #14720, .T. ) ;
#20150 = EDGE_CURVE ( 'NONE', #13576, #1059, #5367, .T. ) ;
#20151 = EDGE_CURVE ( 'NONE', #7199, #500, #16984, .T. ) ;
#20152 = ORIENTED_EDGE ( 'NONE', *, *, #2865, .T. ) ;
#20153 = CARTESIAN_POINT ( 'NONE',  ( 2.058799720203610129, 52.21693617655245134, 78.85847600527985435 ) ) ;
#20154 = CARTESIAN_POINT ( 'NONE',  ( 2.043125170982144745, 38.48583871533720213, 93.92996380123798872 ) ) ;
#20155 = EDGE_LOOP ( 'NONE', ( #20681, #16734, #11542, #155 ) ) ;
#20156 = CARTESIAN_POINT ( 'NONE',  ( -4.259582575189197584, 50.81418445627816993, 75.97269380145769446 ) ) ;
#20157 = CARTESIAN_POINT ( 'NONE',  ( 5.078534106480070420, 37.34458401757132862, 76.40549045149212759 ) ) ;
#20158 = EDGE_CURVE ( 'NONE', #13483, #20468, #9768, .T. ) ;
#20159 =( BOUNDED_CURVE ( )  B_SPLINE_CURVE ( 3, ( #15048, #1959, #18447, #462 ),
 .UNSPECIFIED., .F., .F. ) 
 B_SPLINE_CURVE_WITH_KNOTS ( ( 4, 4 ),
 ( 4.188790204786391413, 4.300872134317200945 ),
 .UNSPECIFIED. ) 
 CURVE ( )  GEOMETRIC_REPRESENTATION_ITEM ( )  RATIONAL_B_SPLINE_CURVE ( ( 1.000000000000000000, 0.9989534107080366709, 0.9989534107080366709, 1.000000000000000000 ) ) 
 REPRESENTATION_ITEM ( '' )  );
#20160 = CARTESIAN_POINT ( 'NONE',  ( 4.454354847297358866, 39.79502961122975790, 90.11785626197793420 ) ) ;
#20161 = AXIS2_PLACEMENT_3D ( 'NONE', #9275, #16069, #19148 ) ;
#20162 = CARTESIAN_POINT ( 'NONE',  ( -3.538351547904186045, 36.22109845575787546, 78.30834307773316993 ) ) ;
#20163 = DIRECTION ( 'NONE',  ( 1.000000000000000000, -0.000000000000000000, -0.000000000000000000 ) ) ;
#20164 = DIRECTION ( 'NONE',  ( -1.540237394707284220E-16, -1.793354297423764243E-16, 1.000000000000000000 ) ) ;
#20165 = EDGE_LOOP ( 'NONE', ( #16437, #14223, #12031, #20732 ) ) ;
#20166 = ORIENTED_EDGE ( 'NONE', *, *, #10319, .F. ) ;
#20167 = CARTESIAN_POINT ( 'NONE',  ( 2.119951781669509927, 52.95431670889340836, 76.39978148915828626 ) ) ;
#20168 = ORIENTED_EDGE ( 'NONE', *, *, #8088, .F. ) ;
#20169 = CARTESIAN_POINT ( 'NONE',  ( 6.919062940419317798, 50.37745683356979498, 76.08942471621537607 ) ) ;
#20170 = ADVANCED_FACE ( 'NONE', ( #16253 ), #14648, .T. ) ;
#20171 = DIRECTION ( 'NONE',  ( -1.540237394707284467E-16, -1.793354297423764243E-16, 1.000000000000000000 ) ) ;
#20172 = CARTESIAN_POINT ( 'NONE',  ( -7.244356193800459032, 41.53104495169013433, 78.90520642705492094 ) ) ;
#20173 = VERTEX_POINT ( 'NONE', #16463 ) ;
#20174 = EDGE_CURVE ( 'NONE', #14996, #16593, #6963, .T. ) ;
#20175 = CARTESIAN_POINT ( 'NONE',  ( 6.324981017461724697, 49.90226621375084193, 79.13556070921569585 ) ) ;
#20176 = VERTEX_POINT ( 'NONE', #13269 ) ;
#20177 = CARTESIAN_POINT ( 'NONE',  ( -2.055347584452832166, 51.31805217249780782, 72.45432679953087529 ) ) ;
#20178 = CARTESIAN_POINT ( 'NONE',  ( -6.753843712027886248, 40.38066566033639759, 76.16022115247204738 ) ) ;
#20179 = CARTESIAN_POINT ( 'NONE',  ( 8.529329397667178014, 40.35666579756309602, 75.60774188071792423 ) ) ;
#20180 = DIRECTION ( 'NONE',  ( 0.5773502691896226224, 0.5773502691896224004, -0.5773502691896322814 ) ) ;
#20181 = CARTESIAN_POINT ( 'NONE',  ( 0.5221537403065097394, 44.16218137147969003, 111.0905869729573681 ) ) ;
#20182 = PLANE ( 'NONE',  #9616 ) ;
#20183 = CARTESIAN_POINT ( 'NONE',  ( 5.568489401881125289, 48.03437091500646261, 94.32058880123798872 ) ) ;
#20184 = CARTESIAN_POINT ( 'NONE',  ( 8.831661421392389855, 41.26277405225351202, 75.98994273744924044 ) ) ;
#20185 = LINE ( 'NONE', #17005, #9517 ) ;
#20186 = CARTESIAN_POINT ( 'NONE',  ( 5.308657174530699407, 50.64216575474390680, 75.36022115247205022 ) ) ;
#20187 = CARTESIAN_POINT ( 'NONE',  ( -4.500660556396669065, 42.81632233694663370, 91.82058880294496817 ) ) ;
#20188 = LINE ( 'NONE', #5618, #2119 ) ;
#20189 = CARTESIAN_POINT ( 'NONE',  ( 8.374367785101570760, 41.81231160194442964, 78.68229860608910542 ) ) ;
#20190 = ORIENTED_EDGE ( 'NONE', *, *, #16162, .F. ) ;
#20191 = CARTESIAN_POINT ( 'NONE',  ( 5.202885763635528349, 50.89499265101085967, 76.90580938776616904 ) ) ;
#20192 = LINE ( 'NONE', #10444, #3781 ) ;
#20193 = CARTESIAN_POINT ( 'NONE',  ( -4.434148273901388215, 50.69479882682543348, 78.79940573867644105 ) ) ;
#20194 = CARTESIAN_POINT ( 'NONE',  ( 1.352400422481993658, 50.46853102219002096, 95.72683880123798872 ) ) ;
#20195 = CARTESIAN_POINT ( 'NONE',  ( 11.22215374030650281, 42.96218137147968008, 61.40715055817103263 ) ) ;
#20196 = CARTESIAN_POINT ( 'NONE',  ( 23.03948732994508575, 43.16218137147968292, 78.30433879953099563 ) ) ;
#20197 = LINE ( 'NONE', #10765, #19421 ) ;
#20198 = CARTESIAN_POINT ( 'NONE',  ( 5.487513352913315323, 50.68176937092437839, 77.98758453411963387 ) ) ;
#20199 = ORIENTED_EDGE ( 'NONE', *, *, #1405, .T. ) ;
#20200 = ORIENTED_EDGE ( 'NONE', *, *, #2882, .T. ) ;
#20201 = CARTESIAN_POINT ( 'NONE',  ( 6.502546507733397263, 49.77243851915681461, 77.06293235403589392 ) ) ;
#20202 = FACE_OUTER_BOUND ( 'NONE', #8790, .T. ) ;
#20203 = CARTESIAN_POINT ( 'NONE',  ( 31.22215374030650281, 45.56218137147968861, 72.80433879953100984 ) ) ;
#20204 = CARTESIAN_POINT ( 'NONE',  ( -5.154188915835984375, 42.64120994080404614, 94.86746380123797451 ) ) ;
#20205 = CARTESIAN_POINT ( 'NONE',  ( 5.561792858816290597, 51.38001756867608094, 76.94115191089467487 ) ) ;
#20206 = CARTESIAN_POINT ( 'NONE',  ( 2.091368541865487707, 52.21063245889819626, 72.45433879953087342 ) ) ;
#20207 = CARTESIAN_POINT ( 'NONE',  ( 4.987494971863720927, 47.58855820898865829, 91.27371380294496817 ) ) ;
#20208 = CARTESIAN_POINT ( 'NONE',  ( -7.718146047797494802, 47.26485609621882844, 78.14247693707426379 ) ) ;
#20209 = CARTESIAN_POINT ( 'NONE',  ( -2.416137431568557314, 39.07291177436112406, 91.11746380123798872 ) ) ;
#20210 = LINE ( 'NONE', #2151, #11951 ) ;
#20211 = ORIENTED_EDGE ( 'NONE', *, *, #3883, .T. ) ;
#20212 = CARTESIAN_POINT ( 'NONE',  ( 1.043496195706703267, 52.34607428218648550, 75.38691198841223695 ) ) ;
#20213 = ORIENTED_EDGE ( 'NONE', *, *, #18211, .T. ) ;
#20214 = CARTESIAN_POINT ( 'NONE',  ( 2.522153740306506187, 47.62628298661744708, 77.15433879953100416 ) ) ;
#20215 = CARTESIAN_POINT ( 'NONE',  ( -5.784195910403845176, 44.99242805365518194, 93.38308880123798872 ) ) ;
#20216 = ORIENTED_EDGE ( 'NONE', *, *, #7104, .T. ) ;
#20217 = CARTESIAN_POINT ( 'NONE',  ( 5.052198367669452850, 48.31320248322255395, 94.67308879782399345 ) ) ;
#20218 = DIRECTION ( 'NONE',  ( 0.8043570849667761591, -0.5941461771851692664, 1.733862608106489734E-17 ) ) ;
#20219 = CARTESIAN_POINT ( 'NONE',  ( -3.600277166070542378, 52.03221539514291294, 79.18928797456808866 ) ) ;
#20220 = CARTESIAN_POINT ( 'NONE',  ( 0.6982372515930639345, 52.96044147935328539, 77.40588267440399761 ) ) ;
#20221 = DIRECTION ( 'NONE',  ( 1.110223024625156540E-16, 1.000000000000000000, 5.922860397471808077E-17 ) ) ;
#20222 = CARTESIAN_POINT ( 'NONE',  ( -4.315046395865206108, 37.70882665799790345, 79.54765774203875139 ) ) ;
#20223 = ORIENTED_EDGE ( 'NONE', *, *, #12126, .T. ) ;
#20224 = PLANE ( 'NONE',  #1371 ) ;
#20225 = B_SPLINE_CURVE_WITH_KNOTS ( 'NONE', 3,
 ( #18900, #14108, #13792, #20590, #18800, #15721, #4213, #17201, #819, #10838, #2623, #9233, #13897, #1139, #7627, #12518, #19001, #17409, #8802, #7193, #20169, #20268, #16987, #8917, #5699, #4104, #17102 ),
 .UNSPECIFIED., .F., .F.,
 ( 4, 1, 1, 1, 1, 1, 1, 1, 1, 1, 1, 1, 1, 1, 1, 1, 1, 1, 1, 1, 1, 1, 1, 1, 4 ),
 ( 0.000000000000000000, 0.05959187408140657199, 0.1157444014141101180, 0.1691701821137891193, 0.2193251454534784761, 0.2669475916912845692, 0.3117751794269221777, 0.3541065092364359956, 0.3940487965473342680, 0.4318372767115636890, 0.4680493653760790518, 0.5025338411669280081, 0.5356117844586580912, 0.5674765898557931898, 0.5983444621881826020, 0.6284125990791417093, 0.6580179645932986432, 0.6886630208720043722, 0.7222707808379922323, 0.7592609375352028511, 0.7993858191113136780, 0.8438632570080943918, 0.8918964550480946718, 0.9439126001412549982, 1.000000000000000000 ),
 .UNSPECIFIED. ) ;
#20226 = ORIENTED_EDGE ( 'NONE', *, *, #12574, .T. ) ;
#20227 = LINE ( 'NONE', #15465, #17274 ) ;
#20228 = CARTESIAN_POINT ( 'NONE',  ( 4.809763630234642484, 51.93551126624419112, 77.58315289018165117 ) ) ;
#20229 = CARTESIAN_POINT ( 'NONE',  ( 6.680635945739894055, 50.55357325011429026, 77.60602934391619101 ) ) ;
#20230 = EDGE_CURVE ( 'NONE', #18234, #970, #5160, .T. ) ;
#20231 = CARTESIAN_POINT ( 'NONE',  ( 7.753636062665578699, 48.02814353133176439, 75.45433879953087342 ) ) ;
#20232 = CARTESIAN_POINT ( 'NONE',  ( -1.477846259693495146, 47.62628298661744708, 45.55433879953100273 ) ) ;
#20233 = DIRECTION ( 'NONE',  ( 1.402518428993854849E-16, -1.000000000000000000, -1.734723475976787846E-14 ) ) ;
#20234 = CARTESIAN_POINT ( 'NONE',  ( -5.616286711741430793, 44.43019146960381960, 94.98558879782399345 ) ) ;
#20235 = B_SPLINE_CURVE_WITH_KNOTS ( 'NONE', 3,
 ( #4184, #17170, #17271, #5893, #15578, #10907, #13977, #13763, #2693, #9202 ),
 .UNSPECIFIED., .F., .F.,
 ( 4, 2, 2, 2, 4 ),
 ( 8.673617379884035472E-18, 0.0002090038972966693713, 0.0004180077945933300689, 0.0006270116918899907394, 0.0008360155891866514642 ),
 .UNSPECIFIED. ) ;
#20236 = CARTESIAN_POINT ( 'NONE',  ( -4.834768248550900260, 37.17870924967544255, 75.36094808373545106 ) ) ;
#20237 = ORIENTED_EDGE ( 'NONE', *, *, #14440, .F. ) ;
#20238 = CARTESIAN_POINT ( 'NONE',  ( 5.037341483232628647, 37.31725042616477594, 78.79551527011911105 ) ) ;
#20239 = ORIENTED_EDGE ( 'NONE', *, *, #11073, .F. ) ;
#20240 = CARTESIAN_POINT ( 'NONE',  ( -4.186692411740909670, 50.69340894834095934, 75.36056307228784590 ) ) ;
#20241 = EDGE_CURVE ( 'NONE', #16818, #2422, #3529, .T. ) ;
#20242 = CARTESIAN_POINT ( 'NONE',  ( 1.868012774839550749, 39.13936707477651566, 93.07058879953099506 ) ) ;
#20243 = B_SPLINE_SURFACE_WITH_KNOTS ( 'NONE', 3, 1, ( 
 ( #666, #15036 ),
 ( #18125, #5233 ),
 ( #13230, #18223 ),
 ( #13650, #13538 ),
 ( #15251, #3956 ),
 ( #10154, #18542 ),
 ( #10265, #11646 ),
 ( #12062, #2055 ),
 ( #11748, #13338 ),
 ( #10479, #16634 ),
 ( #14919, #343 ),
 ( #5560, #5127 ),
 ( #3544, #16945 ),
 ( #5445, #2371 ),
 ( #16527, #15144 ) ),
 .UNSPECIFIED., .F., .F., .F.,
 ( 4, 1, 1, 1, 1, 1, 1, 1, 1, 1, 1, 1, 4 ),
 ( 2, 2 ),
 ( 0.000000000000000000, 0.1108870962763238432, 0.2118129606631371786, 0.3028473642999697790, 0.3830332280304867831, 0.4564275106387662428, 0.5194274750822647224, 0.5737099057017611692, 0.6206015202827788180, 0.7061516677909073225, 0.7943156106821882556, 0.8900258068991424576, 1.000000000000000000 ),
 ( 0.000000000000000000, 1.000000000000000000 ),
 .UNSPECIFIED. ) ;
#20244 = ORIENTED_EDGE ( 'NONE', *, *, #11861, .T. ) ;
#20245 = CARTESIAN_POINT ( 'NONE',  ( -4.567115856812060670, 47.10047254335474065, 92.21121380123797451 ) ) ;
#20246 = CARTESIAN_POINT ( 'NONE',  ( -4.736700016514431510, 50.30022223374984947, 79.44348587025405095 ) ) ;
#20247 = DIRECTION ( 'NONE',  ( 1.402518428993831676E-16, -1.000000000000000000, 0.000000000000000000 ) ) ;
#20248 = CARTESIAN_POINT ( 'NONE',  ( -4.178163250680730023, 41.13787398766260139, 95.05433879953092458 ) ) ;
#20249 = PLANE ( 'NONE',  #14595 ) ;
#20250 = EDGE_CURVE ( 'NONE', #5501, #4681, #16244, .T. ) ;
#20251 = EDGE_LOOP ( 'NONE', ( #18785, #13150, #18358, #16296, #20353, #997, #17786, #4281, #17489, #1664, #5998, #10869 ) ) ;
#20252 = FACE_OUTER_BOUND ( 'NONE', #10252, .T. ) ;
#20253 = ORIENTED_EDGE ( 'NONE', *, *, #3499, .F. ) ;
#20254 = CARTESIAN_POINT ( 'NONE',  ( 0.7518033122594925954, 52.35898226866432026, 77.43632519350985888 ) ) ;
#20255 = CARTESIAN_POINT ( 'NONE',  ( -1.123656915330052408, 35.37488560990637865, 76.16022115247204738 ) ) ;
#20256 = EDGE_CURVE ( 'NONE', #1086, #11013, #3674, .T. ) ;
#20257 = CARTESIAN_POINT ( 'NONE',  ( -4.567115856812060670, 47.10047254335474065, 90.80496380123797451 ) ) ;
#20258 = EDGE_CURVE ( 'NONE', #15837, #18617, #7113, .T. ) ;
#20259 = AXIS2_PLACEMENT_3D ( 'NONE', #7616, #5686, #4404 ) ;
#20260 = ITEM_DEFINED_TRANSFORMATION ( 'NONE', 'NONE', #5447,  #18366 ) ;
#20261 = DIRECTION ( 'NONE',  ( 1.540237394707284220E-16, 1.793354297423764243E-16, -1.000000000000000000 ) ) ;
#20262 = FACE_OUTER_BOUND ( 'NONE', #12505, .T. ) ;
#20263 = DIRECTION ( 'NONE',  ( 1.540237394707284220E-16, 1.793354297423764243E-16, -1.000000000000000000 ) ) ;
#20264 = ORIENTED_EDGE ( 'NONE', *, *, #3138, .T. ) ;
#20265 = EDGE_CURVE ( 'NONE', #10795, #4554, #7813, .T. ) ;
#20266 = CARTESIAN_POINT ( 'NONE',  ( 2.120942209650837018, 52.95430889900478633, 76.48963291717792856 ) ) ;
#20267 = ORIENTED_EDGE ( 'NONE', *, *, #16099, .F. ) ;
#20268 = CARTESIAN_POINT ( 'NONE',  ( 6.934807254081542638, 50.36582714328714871, 76.18099276316716839 ) ) ;
#20269 = CARTESIAN_POINT ( 'NONE',  ( 0.3642233646226559762, 52.96732492115798152, 77.51213090161979835 ) ) ;
#20270 = CARTESIAN_POINT ( 'NONE',  ( 5.568489401881125289, 48.03437091500646261, 90.57058880123798872 ) ) ;
#20271 = CARTESIAN_POINT ( 'NONE',  ( -3.448085832972781262, 52.14096574969422448, 75.97742918362793318 ) ) ;
#20272 = ORIENTED_EDGE ( 'NONE', *, *, #17676, .F. ) ;
#20273 = AXIS2_PLACEMENT_3D ( 'NONE', #12163, #15358, #554 ) ;
#20274 = CARTESIAN_POINT ( 'NONE',  ( 6.195785479992719225, 49.99769775296549312, 79.28554042632779897 ) ) ;
#20275 = ORIENTED_EDGE ( 'NONE', *, *, #3277, .T. ) ;
#20276 = LINE ( 'NONE', #6027, #18618 ) ;
#20277 =( BOUNDED_CURVE ( )  B_SPLINE_CURVE ( 2, ( #11109, #14701, #9508, #4686, #1736, #6497, #6709, #12790, #124 ),
 .UNSPECIFIED., .F., .F. ) 
 B_SPLINE_CURVE_WITH_KNOTS ( ( 3, 2, 2, 2, 3 ),
 ( 0.6423390146554854852, 0.6562500000000000000, 0.6875000000000000000, 0.7187500000000000000, 0.7325704129817647292 ),
 .UNSPECIFIED. ) 
 CURVE ( )  GEOMETRIC_REPRESENTATION_ITEM ( )  RATIONAL_B_SPLINE_CURVE ( ( 0.9623977609649205789, 0.9661148573551012753, 1.000000000000000000, 0.9238795325112867385, 1.000000000000000000, 0.9238795325112867385, 1.000000000000000000, 0.9663354784941116105, 0.9624474427510953944 ) ) 
 REPRESENTATION_ITEM ( '' )  );
#20278 = CARTESIAN_POINT ( 'NONE',  ( 0.5221537403065015237, 48.36218137147969287, 92.45433879953097289 ) ) ;
#20279 = CARTESIAN_POINT ( 'NONE',  ( -4.009385194876760927, 46.27527268018315709, 90.76683879953097289 ) ) ;
#20280 = CARTESIAN_POINT ( 'NONE',  ( 5.487860080568270682, 37.63670891835880639, 77.55534468517188884 ) ) ;
#20281 = CARTESIAN_POINT ( 'NONE',  ( 4.142539520959306110, 51.50352989135271997, 77.22170381446332499 ) ) ;
#20282 = PLANE ( 'NONE',  #5869 ) ;
#20283 = DIRECTION ( 'NONE',  ( -1.334402673828313339E-16, -1.619179559944692391E-32, 1.000000000000000000 ) ) ;
#20284 = CARTESIAN_POINT ( 'NONE',  ( 1.652727357819364640, 35.35299279957455809, 75.45433879953087342 ) ) ;
#20285 = ADVANCED_FACE ( 'NONE', ( #3882 ), #13568, .F. ) ;
#20286 = CARTESIAN_POINT ( 'NONE',  ( 0.8383918983349099019, 52.95649870062635500, 78.71055905107655803 ) ) ;
#20287 = CARTESIAN_POINT ( 'NONE',  ( 4.384086297460604520, 51.32510901764887734, 75.62563104034643402 ) ) ;
#20288 = EDGE_CURVE ( 'NONE', #1015, #19989, #8240, .T. ) ;
#20289 = CARTESIAN_POINT ( 'NONE',  ( -2.077846259693550746, 39.65884927180063357, 94.47683880294496817 ) ) ;
#20290 = DIRECTION ( 'NONE',  ( -1.000000000000000000, 0.000000000000000000, 0.000000000000000000 ) ) ;
#20291 = EDGE_CURVE ( 'NONE', #14218, #11138, #2192, .T. ) ;
#20292 = CARTESIAN_POINT ( 'NONE',  ( 8.322267033824909177, 41.65616234515825056, 78.92561463894257656 ) ) ;
#20293 = EDGE_CURVE ( 'NONE', #3130, #19551, #5480, .T. ) ;
#20294 = EDGE_CURVE ( 'NONE', #12584, #13048, #15171, .T. ) ;
#20295 = ORIENTED_EDGE ( 'NONE', *, *, #17932, .T. ) ;
#20296 = DIRECTION ( 'NONE',  ( 0.000000000000000000, -0.000000000000000000, 1.000000000000000000 ) ) ;
#20297 = CARTESIAN_POINT ( 'NONE',  ( 8.124283007755586539, 44.40224511508533567, 72.45432679953087529 ) ) ;
#20298 = CARTESIAN_POINT ( 'NONE',  ( 2.350558581813033232, 49.87752504164860312, 77.32593395802449265 ) ) ;
#20299 = CARTESIAN_POINT ( 'NONE',  ( -5.784195910403845176, 44.99242805365518194, 93.53933880123797451 ) ) ;
#20300 = VECTOR ( 'NONE', #19476, 1000.000000000000000 ) ;
#20301 = CARTESIAN_POINT ( 'NONE',  ( -4.891140504938443989, 37.22034916465592858, 76.21310604893328389 ) ) ;
#20302 = CARTESIAN_POINT ( 'NONE',  ( -7.527012383044476174, 42.86795482616098951, 79.17794681948264213 ) ) ;
#20303 = CARTESIAN_POINT ( 'NONE',  ( 8.621331711279447418, 42.87908309907099635, 77.81705000150257945 ) ) ;
#20304 = CARTESIAN_POINT ( 'NONE',  ( 0.5221537403065005245, 44.16218137147968292, 82.45433879953087342 ) ) ;
#20305 = EDGE_LOOP ( 'NONE', ( #5734, #6234, #5449, #6532, #6671, #10992, #18126 ) ) ;
#20306 = ORIENTED_EDGE ( 'NONE', *, *, #15237, .T. ) ;
#20307 = CARTESIAN_POINT ( 'NONE',  ( 8.597226904264964276, 42.92457698268714239, 79.03485483908291087 ) ) ;
#20308 = DIRECTION ( 'NONE',  ( 0.3165065846431829311, 0.9485903129789527988, 2.188653791613874255E-16 ) ) ;
#20309 = LINE ( 'NONE', #13831, #15027 ) ;
#20310 = CARTESIAN_POINT ( 'NONE',  ( 0.4222355217934689042, 52.36159922174551440, 78.89164400207971539 ) ) ;
#20311 = CARTESIAN_POINT ( 'NONE',  ( -4.007284936692978583, 40.69155966471626584, 95.05433879953098142 ) ) ;
#20312 = CARTESIAN_POINT ( 'NONE',  ( 8.468902854075459175, 42.53998166354323018, 78.05372954401303787 ) ) ;
#20313 = CARTESIAN_POINT ( 'NONE',  ( 6.722153740306509917, 44.16218137147969003, 92.55433879953098142 ) ) ;
#20314 = VECTOR ( 'NONE', #6857, 1000.000000000000227 ) ;
#20315 = CARTESIAN_POINT ( 'NONE',  ( -4.486751758304120763, 51.39877310743911210, 75.98707017319573254 ) ) ;
#20316 = CARTESIAN_POINT ( 'NONE',  ( -6.857750647227540242, 47.71699458730062560, 78.32480289656686523 ) ) ;
#20317 = ADVANCED_FACE ( 'NONE', ( #20482 ), #8792, .T. ) ;
#20318 = CARTESIAN_POINT ( 'NONE',  ( -5.506217236748579325, 38.61068806573513257, 78.67637590524894620 ) ) ;
#20319 = B_SPLINE_CURVE_WITH_KNOTS ( 'NONE', 3,
 ( #2155, #10040, #8654, #16312, #18314, #14807 ),
 .UNSPECIFIED., .F., .F.,
 ( 4, 2, 4 ),
 ( 0.000000000000000000, 0.001381092432504990586, 0.002762184865009981172 ),
 .UNSPECIFIED. ) ;
#20320 = CARTESIAN_POINT ( 'NONE',  ( 6.882377701754223587, 37.89119233413698140, 76.59354538285809610 ) ) ;
#20321 = ORIENTED_EDGE ( 'NONE', *, *, #3917, .F. ) ;
#20322 = CARTESIAN_POINT ( 'NONE',  ( 0.6841097403222727857, 52.36108336152096854, 75.36125153625724238 ) ) ;
#20323 = ORIENTED_EDGE ( 'NONE', *, *, #6604, .T. ) ;
#20324 = CARTESIAN_POINT ( 'NONE',  ( -4.244931195431495219, 50.82465379583177167, 78.93669174070734584 ) ) ;
#20325 = CARTESIAN_POINT ( 'NONE',  ( 6.828503391016846891, 43.33193468930419101, 91.50808880123798872 ) ) ;
#20326 = VERTEX_POINT ( 'NONE', #7181 ) ;
#20327 = PLANE ( 'NONE',  #9628 ) ;
#20328 = VECTOR ( 'NONE', #5775, 1000.000000000000000 ) ;
#20329 = LINE ( 'NONE', #10585, #6386 ) ;
#20330 = CARTESIAN_POINT ( 'NONE',  ( -3.013797660541937873, 51.53151659513010685, 78.93778436892569061 ) ) ;
#20331 = CARTESIAN_POINT ( 'NONE',  ( 2.522153740306494640, 49.81903562097208749, 75.21119304902340730 ) ) ;
#20332 = CARTESIAN_POINT ( 'NONE',  ( 5.739698376139652503, 51.24860592950068394, 77.28905211432859801 ) ) ;
#20333 = CARTESIAN_POINT ( 'NONE',  ( -3.160478584913959388, 36.85599392487655734, 78.92082147625116306 ) ) ;
#20334 = ORIENTED_EDGE ( 'NONE', *, *, #13550, .F. ) ;
#20335 = CARTESIAN_POINT ( 'NONE',  ( 8.215275734490949944, 41.32388948499509240, 77.23539183544390596 ) ) ;
#20336 = ORIENTED_EDGE ( 'NONE', *, *, #12878, .F. ) ;
#20337 = ADVANCED_FACE ( 'NONE', ( #18467 ), #10406, .F. ) ;
#20338 = CARTESIAN_POINT ( 'NONE',  ( 1.403788643848841389, 39.16218137147969003, 94.95233169107483207 ) ) ;
#20339 = CARTESIAN_POINT ( 'NONE',  ( -6.782631326057145138, 43.38225751353197523, 75.45433879953087342 ) ) ;
#20340 = FACE_OUTER_BOUND ( 'NONE', #7700, .T. ) ;
#20341 = DIRECTION ( 'NONE',  ( 1.402518428993831676E-16, -1.000000000000000000, 0.000000000000000000 ) ) ;
#20342 = CARTESIAN_POINT ( 'NONE',  ( -7.616632640849319458, 40.81216055894036288, 77.06254053058707143 ) ) ;
#20343 = DIRECTION ( 'NONE',  ( 0.000000000000000000, 0.000000000000000000, 1.000000000000000000 ) ) ;
#20344 = CARTESIAN_POINT ( 'NONE',  ( 3.394633603133437205, 39.16678578622979501, 95.56538158822176854 ) ) ;
#20345 = DIRECTION ( 'NONE',  ( 1.196361017915039239E-16, 0.000000000000000000, -1.000000000000000000 ) ) ;
#20346 = AXIS2_PLACEMENT_3D ( 'NONE', #18164, #16365, #18060 ) ;
#20347 = EDGE_LOOP ( 'NONE', ( #10166, #6589, #16753, #14950 ) ) ;
#20348 = CARTESIAN_POINT ( 'NONE',  ( 4.100026115879673583, 51.54044873340893673, 76.58963291717793709 ) ) ;
#20349 = ORIENTED_EDGE ( 'NONE', *, *, #11741, .F. ) ;
#20350 = AXIS2_PLACEMENT_3D ( 'NONE', #11164, #20821, #7858 ) ;
#20351 = DIRECTION ( 'NONE',  ( -1.402518428993831183E-16, 1.000000000000000000, -3.469446951953617640E-16 ) ) ;
#20352 = CARTESIAN_POINT ( 'NONE',  ( 1.868012774839550749, 39.13936707477651566, 91.82058879953099506 ) ) ;
#20353 = ORIENTED_EDGE ( 'NONE', *, *, #16339, .T. ) ;
#20354 = EDGE_CURVE ( 'NONE', #8963, #1387, #8162, .T. ) ;
#20355 = CIRCLE ( 'NONE', #12222, 4.000000000000003553 ) ;
#20356 = CARTESIAN_POINT ( 'NONE',  ( -2.416137431568557314, 39.07291177436112406, 93.77371380123797451 ) ) ;
#20357 = CARTESIAN_POINT ( 'NONE',  ( 2.921181103050038086, 49.30691215337508737, 94.59496379782397923 ) ) ;
#20358 = CYLINDRICAL_SURFACE ( 'NONE', #9283, 6.000000000000001776 ) ;
#20359 = EDGE_LOOP ( 'NONE', ( #8642, #7026, #17704 ) ) ;
#20360 = DIRECTION ( 'NONE',  ( 3.154042683594179047E-15, 0.000000000000000000, -1.000000000000000000 ) ) ;
#20361 = DIRECTION ( 'NONE',  ( -0.9999689119394086223, 0.007885122365278607326, -1.526048693634347968E-16 ) ) ;
#20362 = ORIENTED_EDGE ( 'NONE', *, *, #2220, .T. ) ;
#20363 = CYLINDRICAL_SURFACE ( 'NONE', #16994, 8.199999999999995737 ) ;
#20364 = AXIS2_PLACEMENT_3D ( 'NONE', #280, #3791, #183 ) ;
#20365 = CARTESIAN_POINT ( 'NONE',  ( 0.8247868767332566797, 52.35233939957169014, 78.75172105370583608 ) ) ;
#20366 = EDGE_LOOP ( 'NONE', ( #5459, #21008, #20639, #2685 ) ) ;
#20367 = CARTESIAN_POINT ( 'NONE',  ( -3.063797695301091473, 40.22636611860890810, 92.45433879953094447 ) ) ;
#20368 = CARTESIAN_POINT ( 'NONE',  ( 5.076572431691917409, 37.34329067111212197, 76.70433879953087342 ) ) ;
#20369 = EDGE_CURVE ( 'NONE', #6553, #4848, #7067, .T. ) ;
#20370 = AXIS2_PLACEMENT_3D ( 'NONE', #3670, #5053, #10182 ) ;
#20371 = APPLICATION_PROTOCOL_DEFINITION ( 'draft international standard', 'automotive_design', 1998, #5175 ) ;
#20372 = CARTESIAN_POINT ( 'NONE',  ( 5.427951760950261217, 36.85191280677083370, 76.67247627436783830 ) ) ;
#20374 = ADVANCED_FACE ( 'NONE', ( #12195 ), #10622, .T. ) ;
#20373 = AXIS2_PLACEMENT_3D ( 'NONE', #16330, #19508, #11546 ) ;
#20375 = CARTESIAN_POINT ( 'NONE',  ( 5.464930624430781592, 36.87833654873140432, 76.10043865634602867 ) ) ;
#20376 = CARTESIAN_POINT ( 'NONE',  ( 1.652727357819363974, 35.35299279957455099, 79.45433879953087342 ) ) ;
#20377 = EDGE_LOOP ( 'NONE', ( #14107, #12525, #9432, #19549 ) ) ;
#20378 = CARTESIAN_POINT ( 'NONE',  ( 1.879340735999647682, 52.20337590418190388, 75.75738117569228791 ) ) ;
#20379 = CIRCLE ( 'NONE', #12567, 8.199999999999995737 ) ;
#20380 = ORIENTED_EDGE ( 'NONE', *, *, #13907, .T. ) ;
#20381 = CARTESIAN_POINT ( 'NONE',  ( 1.851481395807866859, 48.14626068599128672, 82.45433879953087342 ) ) ;
#20382 = DIRECTION ( 'NONE',  ( -1.402518428993831676E-16, 1.000000000000000000, -0.000000000000000000 ) ) ;
#20383 = CARTESIAN_POINT ( 'NONE',  ( -4.567115856812060670, 47.10047254335474065, 90.96121380123797451 ) ) ;
#20384 = B_SPLINE_SURFACE_WITH_KNOTS ( 'NONE', 3, 1, ( 
 ( #6654, #1783 ),
 ( #14331, #6235 ),
 ( #2943, #3051 ),
 ( #11261, #8153 ),
 ( #19215, #12738 ),
 ( #6438, #3262 ),
 ( #4630, #3359 ),
 ( #6550, #20902 ),
 ( #13056, #11151 ),
 ( #6333, #13156 ),
 ( #9560, #16043 ),
 ( #1464, #14749 ),
 ( #9449, #7949 ),
 ( #15935, #19427 ),
 ( #12835, #19530 ),
 ( #19315, #4731 ),
 ( #9665, #17732 ),
 ( #4946, #1566 ),
 ( #8051, #9869 ) ),
 .UNSPECIFIED., .F., .F., .F.,
 ( 4, 1, 1, 1, 1, 1, 1, 1, 1, 1, 1, 1, 1, 1, 1, 1, 4 ),
 ( 2, 2 ),
 ( 0.000000000000000000, 0.09593561818428578136, 0.1790132514218915338, 0.2495659677033479074, 0.3103928923273128748, 0.3657232523743771391, 0.4198889549570182789, 0.4761292045875803458, 0.5349114402766786958, 0.5687027968553886037, 0.6100175737345402416, 0.6575813992106814831, 0.7121752348458817439, 0.7738275843818921418, 0.8419112148355063496, 0.9177342363179752383, 1.000000000000000000 ),
 ( 0.000000000000000000, 1.000000000000000000 ),
 .UNSPECIFIED. ) ;
#20385 = CARTESIAN_POINT ( 'NONE',  ( -3.349945445540459588, 52.21109327740445138, 76.66413924479479647 ) ) ;
#20386 = VERTEX_POINT ( 'NONE', #4094 ) ;
#20387 = VECTOR ( 'NONE', #5691, 1000.000000000000000 ) ;
#20388 = VECTOR ( 'NONE', #18669, 1000.000000000000114 ) ;
#20389 = FACE_OUTER_BOUND ( 'NONE', #13746, .T. ) ;
#20390 = B_SPLINE_CURVE_WITH_KNOTS ( 'NONE', 3,
 ( #7634, #9241, #14014, #17205, #2630, #9130 ),
 .UNSPECIFIED., .F., .F.,
 ( 4, 2, 4 ),
 ( 0.000000000000000000, 0.002233127396118993191, 0.004466254792237986382 ),
 .UNSPECIFIED. ) ;
#20391 = VERTEX_POINT ( 'NONE', #7510 ) ;
#20392 = CARTESIAN_POINT ( 'NONE',  ( -1.477846259693492037, 50.16218137147969713, 67.55433879953099563 ) ) ;
#20393 = CARTESIAN_POINT ( 'NONE',  ( 1.658154530501164237, 36.04125148601230677, 72.45433879953085921 ) ) ;
#20394 = CARTESIAN_POINT ( 'NONE',  ( 7.760798028454924946, 40.43451328883516993, 75.74322883085581282 ) ) ;
#20395 = CARTESIAN_POINT ( 'NONE',  ( 5.357400835671676020, 37.53933297990715801, 77.75509786706420812 ) ) ;
#20396 = CARTESIAN_POINT ( 'NONE',  ( -6.972818533526913498, 41.14430689552183651, 79.47750830342025097 ) ) ;
#20397 = DIRECTION ( 'NONE',  ( -1.402518428993831183E-16, 1.000000000000000000, -3.469446951953617640E-16 ) ) ;
#20398 = CARTESIAN_POINT ( 'NONE',  ( 5.568489401881125289, 48.03437091500646261, 95.57058880123798872 ) ) ;
#20399 = DIRECTION ( 'NONE',  ( -0.3165065846431826535, -0.9485903129789529098, -2.188653791613874008E-16 ) ) ;
#20400 = CARTESIAN_POINT ( 'NONE',  ( -5.825614074793430852, 50.44207111495388318, 76.36675183022860836 ) ) ;
#20401 = CARTESIAN_POINT ( 'NONE',  ( 4.334149498405073686, 51.36199531953422337, 75.67068799376596644 ) ) ;
#20402 = EDGE_CURVE ( 'NONE', #14686, #17246, #20034, .T. ) ;
#20403 = CARTESIAN_POINT ( 'NONE',  ( -3.981178359372548492, 46.76218137147973408, 92.91433880294496817 ) ) ;
#20404 = VECTOR ( 'NONE', #5730, 1000.000000000000000 ) ;
#20405 = CARTESIAN_POINT ( 'NONE',  ( -7.291056197748040368, 40.11326154233370289, 78.55231559615423009 ) ) ;
#20406 = ORIENTED_EDGE ( 'NONE', *, *, #20675, .T. ) ;
#20407 = CARTESIAN_POINT ( 'NONE',  ( 8.289318114139261340, 41.55741234261986250, 78.93669174070734584 ) ) ;
#20408 = ORIENTED_EDGE ( 'NONE', *, *, #10844, .T. ) ;
#20409 = CARTESIAN_POINT ( 'NONE',  ( 0.5221537403065009686, 44.16218137147968292, 79.45433879953087342 ) ) ;
#20410 = DIRECTION ( 'NONE',  ( -1.402518428993831183E-16, 1.000000000000000000, -3.469446951953617640E-16 ) ) ;
#20411 = DIRECTION ( 'NONE',  ( 0.000000000000000000, -1.000000000000000000, 0.000000000000000000 ) ) ;
#20412 = DIRECTION ( 'NONE',  ( 0.000000000000000000, -1.000000000000000000, 0.000000000000000000 ) ) ;
#20413 = VECTOR ( 'NONE', #9682, 1000.000000000000114 ) ;
#20414 = EDGE_CURVE ( 'NONE', #14294, #7818, #15497, .T. ) ;
#20415 = PLANE ( 'NONE',  #10908 ) ;
#20416 = CARTESIAN_POINT ( 'NONE',  ( -7.388159386333283507, 42.42885804414905238, 79.45715840112796968 ) ) ;
#20417 = CARTESIAN_POINT ( 'NONE',  ( -1.477846259693493369, 50.16218137147969713, 75.55433879953099563 ) ) ;
#20418 = EDGE_CURVE ( 'NONE', #11503, #9686, #11916, .T. ) ;
#20419 = EDGE_LOOP ( 'NONE', ( #9618, #11783, #8035, #19996 ) ) ;
#20420 = ORIENTED_EDGE ( 'NONE', *, *, #17369, .T. ) ;
#20421 = CARTESIAN_POINT ( 'NONE',  ( 9.353525637756030520, 42.82683421514393274, 78.50890480505780999 ) ) ;
#20422 = DIRECTION ( 'NONE',  ( -0.000000000000000000, -0.000000000000000000, -1.000000000000000000 ) ) ;
#20423 = ADVANCED_FACE ( 'NONE', ( #12507 ), #12715, .F. ) ;
#20424 = CARTESIAN_POINT ( 'NONE',  ( 1.514255888186003984, 52.36218137147968577, 87.21440135111343750 ) ) ;
#20426 = EDGE_CURVE ( 'NONE', #19924, #12487, #20379, .T. ) ;
#20425 = CARTESIAN_POINT ( 'NONE',  ( 0.4034091969759198149, 52.36133432042633729, 78.87521808986805638 ) ) ;
#20427 = FACE_OUTER_BOUND ( 'NONE', #19602, .T. ) ;
#20428 = CARTESIAN_POINT ( 'NONE',  ( 9.222679282817953350, 42.43467938865651945, 77.98843304575544266 ) ) ;
#20429 = CARTESIAN_POINT ( 'NONE',  ( -4.500660556396669065, 42.81632233694663370, 93.07058880294496817 ) ) ;
#20430 = CONICAL_SURFACE ( 'NONE', #11613, 3.200000000000008171, 0.7853981633974533860 ) ;
#20431 = EDGE_CURVE ( 'NONE', #14686, #10889, #1129, .T. ) ;
#20432 = CARTESIAN_POINT ( 'NONE',  ( -4.383473025373058718, 51.47257230871590394, 76.47051527011910821 ) ) ;
#20433 = LINE ( 'NONE', #5862, #11205 ) ;
#20434 = CARTESIAN_POINT ( 'NONE',  ( 4.454354847297358866, 39.79502961122975790, 90.11785626197793420 ) ) ;
#20435 = CARTESIAN_POINT ( 'NONE',  ( -7.986269739301712356, 41.91386901559200595, 79.52730241447633830 ) ) ;
#20436 = ORIENTED_EDGE ( 'NONE', *, *, #487, .F. ) ;
#20437 = CARTESIAN_POINT ( 'NONE',  ( 5.579204724385461667, 50.61252018296998045, 76.96076274685535168 ) ) ;
#20438 = ORIENTED_EDGE ( 'NONE', *, *, #13550, .T. ) ;
#20439 = VECTOR ( 'NONE', #13358, 1000.000000000000000 ) ;
#20440 = CARTESIAN_POINT ( 'NONE',  ( -4.451329120265561379, 50.67716939545568522, 78.45066232894264147 ) ) ;
#20441 = CIRCLE ( 'NONE', #17399, 1.399999999999995026 ) ;
#20442 = CARTESIAN_POINT ( 'NONE',  ( 1.256812508749381774, 49.74246873332880625, 90.17996380294496817 ) ) ;
#20443 = EDGE_LOOP ( 'NONE', ( #3968, #7985, #19363, #6760 ) ) ;
#20444 = CARTESIAN_POINT ( 'NONE',  ( -0.9402972064945576136, 52.21947918594909765, 76.74746709665741662 ) ) ;
#20445 = CARTESIAN_POINT ( 'NONE',  ( -3.154801521863568325, 47.83913663364971569, 95.05433879953098142 ) ) ;
#20446 = CARTESIAN_POINT ( 'NONE',  ( 6.114519447167765520, 37.34250893849451813, 78.36972961004526894 ) ) ;
#20447 = CARTESIAN_POINT ( 'NONE',  ( 1.771153339986181408, 40.36218137147969287, 105.5543387995310098 ) ) ;
#20448 = ADVANCED_FACE ( 'NONE', ( #17398 ), #6109, .T. ) ;
#20449 = CARTESIAN_POINT ( 'NONE',  ( -3.635499589166290679, 36.29285780047638355, 79.01720576857120193 ) ) ;
#20450 = ORIENTED_EDGE ( 'NONE', *, *, #11294, .F. ) ;
#20451 = CARTESIAN_POINT ( 'NONE',  ( 5.683893922249901642, 37.03479970459495263, 77.75763958275959453 ) ) ;
#20452 = CARTESIAN_POINT ( 'NONE',  ( 2.921181103050038974, 49.30691215337508737, 93.34496379782397923 ) ) ;
#20453 = ORIENTED_EDGE ( 'NONE', *, *, #8083, .T. ) ;
#20454 = FACE_OUTER_BOUND ( 'NONE', #17459, .T. ) ;
#20455 = CARTESIAN_POINT ( 'NONE',  ( 10.77494014480653917, 42.96218137147968008, 58.20715055817105110 ) ) ;
#20456 = CARTESIAN_POINT ( 'NONE',  ( -7.061235947027594051, 47.28415677317426713, 78.95240186183670517 ) ) ;
#20457 = PLANE ( 'NONE',  #15937 ) ;
#20458 = AXIS2_PLACEMENT_3D ( 'NONE', #2954, #20611, #19134 ) ;
#20459 = CARTESIAN_POINT ( 'NONE',  ( 5.176818351154000020, 40.65164613849449182, 95.64871367200940711 ) ) ;
#20460 = CARTESIAN_POINT ( 'NONE',  ( 6.461625768302495132, 49.81576021970867885, 78.82409288115771062 ) ) ;
#20461 = AXIS2_PLACEMENT_3D ( 'NONE', #14404, #17592, #11537 ) ;
#20462 = ORIENTED_EDGE ( 'NONE', *, *, #7930, .T. ) ;
#20463 = CARTESIAN_POINT ( 'NONE',  ( 8.237563311767338803, 41.40248246318230230, 78.88950904781501094 ) ) ;
#20464 = ORIENTED_EDGE ( 'NONE', *, *, #9968, .F. ) ;
#20465 = CARTESIAN_POINT ( 'NONE',  ( -5.955451856753747109, 38.00651308716548726, 77.05433879953086773 ) ) ;
#20466 = CARTESIAN_POINT ( 'NONE',  ( 4.613683346302097199, 40.84891852973634485, 90.69696562749766144 ) ) ;
#20467 = CARTESIAN_POINT ( 'NONE',  ( 4.540684532156292086, 52.13426915682742901, 76.47586842453881673 ) ) ;
#20468 = VERTEX_POINT ( 'NONE', #18991 ) ;
#20469 = CARTESIAN_POINT ( 'NONE',  ( -0.3080929418689875576, 37.85583172076933778, 95.10183880123796030 ) ) ;
#20470 = CARTESIAN_POINT ( 'NONE',  ( -1.219056181836354558, 49.77488197367695477, 94.40612966814926210 ) ) ;
#20471 = ORIENTED_EDGE ( 'NONE', *, *, #18621, .T. ) ;
#20473 = B_SPLINE_CURVE_WITH_KNOTS ( 'NONE', 3,
 ( #2003, #3800, #12016, #11796, #18490, #5182, #18271, #11905, #8500, #15091 ),
 .UNSPECIFIED., .F., .F.,
 ( 4, 2, 2, 2, 4 ),
 ( 0.000000000000000000, 0.0002779176703289528566, 0.0003473970879111939439, 0.0004168765054934349770, 0.0005558353406579482139 ),
 .UNSPECIFIED. ) ;
#20472 = CIRCLE ( 'NONE', #6205, 1.399999999999995026 ) ;
#20474 = CARTESIAN_POINT ( 'NONE',  ( 6.467096401101858127, 37.59444752110963606, 78.28436300994860630 ) ) ;
#20475 = DIRECTION ( 'NONE',  ( 3.211742425186504723E-16, -5.922860397471811774E-17, 1.000000000000000000 ) ) ;
#20476 = AXIS2_PLACEMENT_3D ( 'NONE', #15308, #723, #7204 ) ;
#20477 = ORIENTED_EDGE ( 'NONE', *, *, #6345, .T. ) ;
#20478 = CARTESIAN_POINT ( 'NONE',  ( 1.324134094588556687, 52.32343890518788498, 79.46661588923706177 ) ) ;
#20479 = CARTESIAN_POINT ( 'NONE',  ( -0.3080929418689875576, 37.85583172076933778, 92.60183880123797451 ) ) ;
#20480 = ORIENTED_EDGE ( 'NONE', *, *, #14285, .T. ) ;
#20481 = CARTESIAN_POINT ( 'NONE',  ( -4.392964107369902393, 50.72663347050586680, 79.54348553280554768 ) ) ;
#20482 = FACE_OUTER_BOUND ( 'NONE', #17253, .T. ) ;
#20483 = CARTESIAN_POINT ( 'NONE',  ( 2.921181103050038530, 49.30691215337508737, 93.50121379782399345 ) ) ;
#20484 = CARTESIAN_POINT ( 'NONE',  ( 5.658108625003792191, 37.01637447524286273, 75.97198585835440099 ) ) ;
#20485 = CARTESIAN_POINT ( 'NONE',  ( 5.239968004300939342, 50.86462114820943725, 78.68193220087633222 ) ) ;
#20486 = ADVANCED_FACE ( 'NONE', ( #19193 ), #9224, .T. ) ;
#20487 = AXIS2_PLACEMENT_3D ( 'NONE', #12426, #20497, #20596 ) ;
#20488 = DIRECTION ( 'NONE',  ( 0.000000000000000000, 2.891205793294680792E-16, 1.000000000000000000 ) ) ;
#20489 = VERTEX_POINT ( 'NONE', #2717 ) ;
#20490 = CARTESIAN_POINT ( 'NONE',  ( 0.9729319684334255536, 52.96336138165750640, 75.37848164766056414 ) ) ;
#20491 = VERTEX_POINT ( 'NONE', #3025 ) ;
#20492 = CARTESIAN_POINT ( 'NONE',  ( 14.52215374030650175, 44.16218137147969003, 105.5543387995309956 ) ) ;
#20493 = CARTESIAN_POINT ( 'NONE',  ( -0.9424755721682813725, 52.23032563868695632, 76.73465573240828519 ) ) ;
#20494 = CARTESIAN_POINT ( 'NONE',  ( -4.567115856812060670, 47.10047254335474065, 92.21121380123797451 ) ) ;
#20495 = EDGE_LOOP ( 'NONE', ( #3545, #15236, #2729, #5338, #19144 ) ) ;
#20496 = ORIENTED_EDGE ( 'NONE', *, *, #1045, .T. ) ;
#20497 = DIRECTION ( 'NONE',  ( -1.193617070626243484E-16, -1.000000000000000000, -0.000000000000000000 ) ) ;
#20498 = VERTEX_POINT ( 'NONE', #17291 ) ;
#20499 = CARTESIAN_POINT ( 'NONE',  ( 4.759830266884094385, 51.05838002508453144, 79.48101422306089603 ) ) ;
#20500 = DIRECTION ( 'NONE',  ( -0.9585804129707224952, -0.2848220354341971516, -1.987228219138359058E-16 ) ) ;
#20501 = CARTESIAN_POINT ( 'NONE',  ( 8.491906929791015912, 40.24450828730113727, 75.69429397690826988 ) ) ;
#20502 = AXIS2_PLACEMENT_3D ( 'NONE', #5636, #7447, #14045 ) ;
#20503 = ORIENTED_EDGE ( 'NONE', *, *, #12363, .F. ) ;
#20504 = CARTESIAN_POINT ( 'NONE',  ( -5.160557796315993428, 37.41935686500602287, 77.90139762306027649 ) ) ;
#20505 = FACE_OUTER_BOUND ( 'NONE', #19033, .T. ) ;
#20506 = LINE ( 'NONE', #5937, #16306 ) ;
#20507 = CARTESIAN_POINT ( 'NONE',  ( -0.9988176903691428077, 49.83852402762217082, 90.80496380123797451 ) ) ;
#20508 = CARTESIAN_POINT ( 'NONE',  ( 3.117507734380600137, 51.94062193790708903, 80.45433879953087342 ) ) ;
#20509 = CARTESIAN_POINT ( 'NONE',  ( 3.948530577815479337, 39.69684013992245752, 94.71121380294498238 ) ) ;
#20510 = EDGE_CURVE ( 'NONE', #18041, #2157, #10139, .T. ) ;
#20511 = CARTESIAN_POINT ( 'NONE',  ( -0.8237052942265477018, 49.18499566818285018, 90.25808880294496817 ) ) ;
#20512 = ADVANCED_FACE ( 'NONE', ( #9424 ), #15913, .F. ) ;
#20513 = CARTESIAN_POINT ( 'NONE',  ( -7.833772919943922552, 41.39643022996011723, 79.54647314732444841 ) ) ;
#20514 = CARTESIAN_POINT ( 'NONE',  ( 8.950841833175557483, 41.61996530703199682, 78.68229860608910542 ) ) ;
#20515 = AXIS2_PLACEMENT_3D ( 'NONE', #9614, #4897, #22 ) ;
#20516 = VERTEX_POINT ( 'NONE', #6215 ) ;
#20517 = CARTESIAN_POINT ( 'NONE',  ( -7.609845089999874190, 43.10833364818387992, 76.06610350541322418 ) ) ;
#20518 = CARTESIAN_POINT ( 'NONE',  ( -4.792503378000012582, 37.91763016944491227, 77.90139762306027649 ) ) ;
#20519 = CARTESIAN_POINT ( 'NONE',  ( -4.453436368711328974, 50.68011839687689957, 78.45066232894264147 ) ) ;
#20520 = SURFACE_SIDE_STYLE ('',( #19038 ) ) ;
#20521 = CARTESIAN_POINT ( 'NONE',  ( -8.048135109371418849, 42.06361933714661916, 79.49764826322659417 ) ) ;
#20522 = CARTESIAN_POINT ( 'NONE',  ( -7.677846259693485109, 51.36218137147968577, 93.55433879953098142 ) ) ;
#20523 = EDGE_CURVE ( 'NONE', #18484, #17717, #3389, .T. ) ;
#20524 = ORIENTED_EDGE ( 'NONE', *, *, #16497, .F. ) ;
#20525 = CARTESIAN_POINT ( 'NONE',  ( -4.483923651454749582, 37.66761685267757542, 78.88462034471059781 ) ) ;
#20526 = CARTESIAN_POINT ( 'NONE',  ( -3.681032862722696031, 36.32649139546035855, 79.10742496273583413 ) ) ;
#20527 = CARTESIAN_POINT ( 'NONE',  ( 35.92215374030650565, 47.36218137147962892, 93.55433879953098142 ) ) ;
#20528 = CARTESIAN_POINT ( 'NONE',  ( 5.873343927958857513, 51.14988734394304970, 77.25083512729199242 ) ) ;
#20529 = CARTESIAN_POINT ( 'NONE',  ( 5.613949991644618720, 51.34149119567325670, 78.06835901908682729 ) ) ;
#20530 = CARTESIAN_POINT ( 'NONE',  ( -4.084259173939017273, 50.94606869312387687, 78.87053299850630594 ) ) ;
#20531 = DIRECTION ( 'NONE',  ( -1.000000000000000000, 1.110223024625156540E-16, 6.575695984913707633E-33 ) ) ;
#20532 = ADVANCED_FACE ( 'NONE', ( #1540 ), #8025, .T. ) ;
#20533 = EDGE_CURVE ( 'NONE', #8020, #9071, #19692, .T. ) ;
#20534 = EDGE_CURVE ( 'NONE', #17982, #10889, #7561, .T. ) ;
#20535 = CARTESIAN_POINT ( 'NONE',  ( -4.423683986466107498, 51.44383902813605403, 76.03815620566271605 ) ) ;
#20536 = ORIENTED_EDGE ( 'NONE', *, *, #7927, .T. ) ;
#20537 = CARTESIAN_POINT ( 'NONE',  ( 5.611423337425062385, 41.22389019960463230, 92.67996380123798872 ) ) ;
#20538 = CARTESIAN_POINT ( 'NONE',  ( 0.7364379940111278611, 52.35940638163580019, 78.88801353106350689 ) ) ;
#20539 = ORIENTED_EDGE ( 'NONE', *, *, #19651, .F. ) ;
#20540 = EDGE_CURVE ( 'NONE', #18483, #8749, #11939, .T. ) ;
#20541 = CARTESIAN_POINT ( 'NONE',  ( 2.075723384514267966, 52.21368374790338152, 76.12915149413191784 ) ) ;
#20542 = VERTEX_POINT ( 'NONE', #6813 ) ;
#20543 = DIRECTION ( 'NONE',  ( -0.7071067811865433539, 0.7071067811865517916, -0.000000000000000000 ) ) ;
#20544 = CARTESIAN_POINT ( 'NONE',  ( 3.122153740306552905, 48.66551347115873227, 91.35183880294498238 ) ) ;
#20545 = ORIENTED_EDGE ( 'NONE', *, *, #17955, .F. ) ;
#20546 = CARTESIAN_POINT ( 'NONE',  ( 0.7901638384306272078, 50.30062182352762079, 94.82933879782399345 ) ) ;
#20547 = LINE ( 'NONE', #9074, #7432 ) ;
#20548 = CARTESIAN_POINT ( 'NONE',  ( 8.206376600211122252, 41.34361096682673065, 77.83369646723784285 ) ) ;
#20549 = DIRECTION ( 'NONE',  ( 0.7071067811865443531, 0.7071067811865506814, -2.453269466693410947E-16 ) ) ;
#20550 = LINE ( 'NONE', #7891, #2272 ) ;
#20551 = DIRECTION ( 'NONE',  ( 3.893792155548169402E-16, 7.183611964723547524E-17, -1.000000000000000000 ) ) ;
#20552 = ORIENTED_EDGE ( 'NONE', *, *, #14085, .T. ) ;
#20553 = DIRECTION ( 'NONE',  ( -1.540237394707284220E-16, -1.793354297423764243E-16, 1.000000000000000000 ) ) ;
#20554 = ORIENTED_EDGE ( 'NONE', *, *, #6375, .F. ) ;
#20555 = CARTESIAN_POINT ( 'NONE',  ( 6.181291377576516588, 50.09645632270179050, 77.70598184265482189 ) ) ;
#20556 = CARTESIAN_POINT ( 'NONE',  ( 4.605781907348109883, 52.08618434805546116, 77.30394856433355244 ) ) ;
#20557 = CARTESIAN_POINT ( 'NONE',  ( -3.350035803220276609, 49.20851703305431357, 95.72683880123798872 ) ) ;
#20558 = CARTESIAN_POINT ( 'NONE',  ( 3.460444912181559474, 49.25145096859824889, 95.49246380123798872 ) ) ;
#20559 = DIRECTION ( 'NONE',  ( 0.000000000000000000, 0.000000000000000000, -1.000000000000000000 ) ) ;
#20560 = CARTESIAN_POINT ( 'NONE',  ( 2.463659247115865369, 38.82793883177424732, 95.53246379782397923 ) ) ;
#20561 = EDGE_CURVE ( 'NONE', #5416, #10073, #5109, .T. ) ;
#20562 = CARTESIAN_POINT ( 'NONE',  ( -5.493714318389447904, 37.66544616749837360, 75.52011153330033721 ) ) ;
#20563 = ORIENTED_EDGE ( 'NONE', *, *, #4186, .F. ) ;
#20564 = EDGE_CURVE ( 'NONE', #15118, #10540, #437, .T. ) ;
#20565 = DIRECTION ( 'NONE',  ( 1.779391786395883536E-16, 5.922860397471806844E-17, -1.000000000000000000 ) ) ;
#20566 = EDGE_CURVE ( 'NONE', #9174, #5774, #10216, .T. ) ;
#20567 = ORIENTED_EDGE ( 'NONE', *, *, #19010, .F. ) ;
#20568 = CARTESIAN_POINT ( 'NONE',  ( 3.357643116058060428, 37.76218137147968434, 96.05433879953096721 ) ) ;
#20569 = CARTESIAN_POINT ( 'NONE',  ( 5.568489401881125289, 48.03437091500646261, 95.57058880123798872 ) ) ;
#20570 = CARTESIAN_POINT ( 'NONE',  ( 11.32022995165976198, 38.96218137147968008, 93.55433879953098142 ) ) ;
#20571 = ORIENTED_EDGE ( 'NONE', *, *, #1848, .T. ) ;
#20572 = FACE_OUTER_BOUND ( 'NONE', #10835, .T. ) ;
#20573 = VERTEX_POINT ( 'NONE', #2144 ) ;
#20574 = CARTESIAN_POINT ( 'NONE',  ( 6.882043956598291601, 37.89095385206773869, 77.31245045813156480 ) ) ;
#20575 = CARTESIAN_POINT ( 'NONE',  ( -5.955451856753747997, 38.00651308716548726, 78.18375056423674607 ) ) ;
#20576 = ORIENTED_EDGE ( 'NONE', *, *, #17449, .T. ) ;
#20577 = DIRECTION ( 'NONE',  ( -5.626130192357176673E-16, -1.831515347669941892E-30, 1.000000000000000000 ) ) ;
#20578 = B_SPLINE_CURVE_WITH_KNOTS ( 'NONE', 3,
 ( #19290, #6104, #1432, #12711, #20775, #4603, #6211, #11124, #17594, #3021, #9528, #16012, #6306, #3131, #12807, #8021, #14507, #6409, #3232, #2057, #5235, #10051, #17908, #9734 ),
 .UNSPECIFIED., .F., .F.,
 ( 4, 2, 2, 2, 2, 2, 2, 2, 2, 2, 2, 4 ),
 ( 0.000000000000000000, 0.001360085407871233776, 0.002040128111806841556, 0.002720170815742449337, 0.004080256223613664898, 0.004760298927549273980, 0.005440341631484881327, 0.006800427039356100357, 0.007480469743291708572, 0.008160512447227315919, 0.009520597855098516735, 0.01088068326296971755 ),
 .UNSPECIFIED. ) ;
#20579 = CARTESIAN_POINT ( 'NONE',  ( 0.5838098620965819219, 52.35423959189261467, 78.93669174070734584 ) ) ;
#20580 = ORIENTED_EDGE ( 'NONE', *, *, #5992, .T. ) ;
#20581 = CARTESIAN_POINT ( 'NONE',  ( -1.677846259693484665, 49.95873206995546667, 54.55433879953099563 ) ) ;
#20582 = CARTESIAN_POINT ( 'NONE',  ( 4.483525963726956221, 47.60918346696958281, 95.05433879953102405 ) ) ;
#20583 = CARTESIAN_POINT ( 'NONE',  ( 0.2541436421823703440, 38.02374091943176637, 94.20433879782400766 ) ) ;
#20584 = CARTESIAN_POINT ( 'NONE',  ( 5.111615301690868307, 37.37278578702127874, 76.10043865634602867 ) ) ;
#20585 = CARTESIAN_POINT ( 'NONE',  ( 8.817118105929894867, 41.21918681320168787, 76.01674029036281866 ) ) ;
#20586 = CARTESIAN_POINT ( 'NONE',  ( -7.259306123653141540, 41.57521370724165877, 78.12833282845913629 ) ) ;
#20587 = ORIENTED_EDGE ( 'NONE', *, *, #523, .F. ) ;
#20588 = CARTESIAN_POINT ( 'NONE',  ( 1.769954653961227198, 52.87349229310958521, 76.95685929568175254 ) ) ;
#20589 = ORIENTED_EDGE ( 'NONE', *, *, #16355, .T. ) ;
#20590 = CARTESIAN_POINT ( 'NONE',  ( 5.963693060521315203, 51.08315007920423056, 75.36814786694185386 ) ) ;
#20591 = DIRECTION ( 'NONE',  ( 1.000000000000000000, 0.000000000000000000, 0.000000000000000000 ) ) ;
#20592 = CARTESIAN_POINT ( 'NONE',  ( 3.460444912181559474, 49.25145096859824889, 91.89871380123798872 ) ) ;
#20593 = ORIENTED_EDGE ( 'NONE', *, *, #8887, .T. ) ;
#20594 = ORIENTED_EDGE ( 'NONE', *, *, #8317, .T. ) ;
#20595 = CARTESIAN_POINT ( 'NONE',  ( -5.368445182934975968, 51.36218137147968577, 95.05433879953098142 ) ) ;
#20596 = DIRECTION ( 'NONE',  ( 1.000000000000000000, 0.000000000000000000, 0.000000000000000000 ) ) ;
#20597 = ORIENTED_EDGE ( 'NONE', *, *, #4140, .F. ) ;
#20598 = CARTESIAN_POINT ( 'NONE',  ( -1.477846259693494702, 50.16218137147969713, 85.55433879953100984 ) ) ;
#20599 = LINE ( 'NONE', #2846, #16311 ) ;
#20600 = DIRECTION ( 'NONE',  ( 0.4999999999999981126, -0.8660254037844397068, -0.000000000000000000 ) ) ;
#20601 = VECTOR ( 'NONE', #11265, 1000.000000000000000 ) ;
#20602 = VERTEX_POINT ( 'NONE', #11627 ) ;
#20603 = CARTESIAN_POINT ( 'NONE',  ( -4.555118767358830922, 36.97214344288710208, 78.05402056118774112 ) ) ;
#20604 = CARTESIAN_POINT ( 'NONE',  ( -6.734383500022516067, 40.39030043969829364, 78.92129748799239053 ) ) ;
#20605 = CARTESIAN_POINT ( 'NONE',  ( -4.719372061707844956, 37.85391995346009963, 79.54051286045766744 ) ) ;
#20606 = CARTESIAN_POINT ( 'NONE',  ( -3.350035803220276609, 49.20851703305431357, 90.88308880123797451 ) ) ;
#20607 = CARTESIAN_POINT ( 'NONE',  ( 25.63948732994508362, 45.16218137147969003, 76.90433879953101837 ) ) ;
#20608 = CARTESIAN_POINT ( 'NONE',  ( -1.077846259693492348, 47.82824192744436687, 53.55433879953100273 ) ) ;
#20609 = EDGE_CURVE ( 'NONE', #188, #16089, #18104, .T. ) ;
#20610 = CARTESIAN_POINT ( 'NONE',  ( -5.835808111729286374, 50.43478682938704338, 76.54939005541714891 ) ) ;
#20611 = DIRECTION ( 'NONE',  ( 5.626130192357176673E-16, 1.831515347669941892E-30, -1.000000000000000000 ) ) ;
#20612 = CARTESIAN_POINT ( 'NONE',  ( -0.1986334453709044101, 52.21160884442346628, 79.43762534667510522 ) ) ;
#20613 = VECTOR ( 'NONE', #2267, 1000.000000000000000 ) ;
#20614 = LINE ( 'NONE', #7754, #11545 ) ;
#20615 = CARTESIAN_POINT ( 'NONE',  ( 5.722153740306500147, 44.16218137147968292, 93.33161078214054385 ) ) ;
#20616 = CARTESIAN_POINT ( 'NONE',  ( 5.619974078175711263, 51.33704144561774996, 76.01203914421944319 ) ) ;
#20617 = CARTESIAN_POINT ( 'NONE',  ( 6.198496396448986090, 45.68315280215533392, 90.49246380123798872 ) ) ;
#20618 = CARTESIAN_POINT ( 'NONE',  ( -7.428991370734761901, 42.55798160200171765, 79.40422342893963048 ) ) ;
#20619 = PLANE ( 'NONE',  #3790 ) ;
#20620 = ORIENTED_EDGE ( 'NONE', *, *, #1930, .F. ) ;
#20621 = CARTESIAN_POINT ( 'NONE',  ( 35.92215374030650565, 47.36218137147962892, 45.55433879953098852 ) ) ;
#20622 = CARTESIAN_POINT ( 'NONE',  ( 2.029186242314200861, 35.35002428291939225, 76.86610350541323555 ) ) ;
#20623 = CARTESIAN_POINT ( 'NONE',  ( 32.72215374030650281, 44.16218137147968292, 87.05433879953099563 ) ) ;
#20624 = CARTESIAN_POINT ( 'NONE',  ( -4.677846259692850950, 45.55551717212265572, 93.90237681315545615 ) ) ;
#20625 = CARTESIAN_POINT ( 'NONE',  ( -7.677846259693485109, 51.36218137147968577, 45.55433879953098852 ) ) ;
#20626 = VECTOR ( 'NONE', #4972, 1000.000000000000227 ) ;
#20627 = DIRECTION ( 'NONE',  ( -1.110223024625156540E-16, -1.000000000000000000, -5.922860397471808077E-17 ) ) ;
#20628 = FACE_BOUND ( 'NONE', #17414, .T. ) ;
#20629 = EDGE_CURVE ( 'NONE', #1372, #2631, #8420, .T. ) ;
#20630 = ORIENTED_EDGE ( 'NONE', *, *, #7826, .F. ) ;
#20631 = LINE ( 'NONE', #18841, #4091 ) ;
#20632 = AXIS2_PLACEMENT_3D ( 'NONE', #20734, #11286, #4763 ) ;
#20633 = CARTESIAN_POINT ( 'NONE',  ( 0.5221537403064990812, 39.96218137147968719, 96.05433879953096721 ) ) ;
#20634 = CARTESIAN_POINT ( 'NONE',  ( -3.075450579529443118, 36.79350905225846446, 77.07727084323215649 ) ) ;
#20635 = ORIENTED_EDGE ( 'NONE', *, *, #3197, .T. ) ;
#20636 = CONICAL_SURFACE ( 'NONE', #3314, 3.200000000000008171, 0.7853981633974533860 ) ;
#20637 = CARTESIAN_POINT ( 'NONE',  ( -7.611372734017126440, 43.12018948500615778, 78.13669174070733447 ) ) ;
#20638 = CARTESIAN_POINT ( 'NONE',  ( 3.122153740306552905, 48.66551347115873227, 90.10183880294498238 ) ) ;
#20639 = ORIENTED_EDGE ( 'NONE', *, *, #1692, .T. ) ;
#20640 = CARTESIAN_POINT ( 'NONE',  ( 4.673174852049362116, 39.63213674411673537, 93.11058879782397923 ) ) ;
#20641 = CARTESIAN_POINT ( 'NONE',  ( 1.868012774839550749, 39.13936707477651566, 94.32058879953099506 ) ) ;
#20642 = CARTESIAN_POINT ( 'NONE',  ( -4.452887004952780892, 50.68053776405899669, 76.33594214506553044 ) ) ;
#20643 = CARTESIAN_POINT ( 'NONE',  ( 10.77494014480653561, 42.76218137147968434, 73.80433879953100984 ) ) ;
#20644 = CARTESIAN_POINT ( 'NONE',  ( 0.8457014337750217159, 52.96360462446077833, 76.19252767286178596 ) ) ;
#20645 = CARTESIAN_POINT ( 'NONE',  ( -4.637383097126855702, 37.03290878947739628, 79.54612747205591461 ) ) ;
#20646 = ORIENTED_EDGE ( 'NONE', *, *, #13153, .F. ) ;
#20647 = DIRECTION ( 'NONE',  ( 0.8136266022444372803, 0.5813877811927012917, 2.295812393977109100E-16 ) ) ;
#20648 = VECTOR ( 'NONE', #2776, 1000.000000000000000 ) ;
#20649 = ORIENTED_EDGE ( 'NONE', *, *, #3385, .F. ) ;
#20650 = CARTESIAN_POINT ( 'NONE',  ( 2.043125170982144745, 38.48583871533720213, 93.77371380123798872 ) ) ;
#20651 = CARTESIAN_POINT ( 'NONE',  ( 2.043125170982144745, 38.48583871533720213, 95.02371380123798872 ) ) ;
#20652 = DIRECTION ( 'NONE',  ( 0.000000000000000000, 2.168404344970984808E-15, -1.000000000000000000 ) ) ;
#20653 = CARTESIAN_POINT ( 'NONE',  ( -4.159821392692165887, 37.43023233986658482, 78.25884081218126198 ) ) ;
#20654 = DIRECTION ( 'NONE',  ( 0.8043570849667761591, -0.5941461771851692664, 1.733862608106489734E-17 ) ) ;
#20655 = ORIENTED_EDGE ( 'NONE', *, *, #9776, .F. ) ;
#20656 = FACE_OUTER_BOUND ( 'NONE', #8488, .T. ) ;
#20657 = AXIS2_PLACEMENT_3D ( 'NONE', #20132, #2382, #8882 ) ;
#20658 = ORIENTED_EDGE ( 'NONE', *, *, #9892, .T. ) ;
#20659 = CARTESIAN_POINT ( 'NONE',  ( 7.680032241523796266, 40.16158449578585277, 77.13595644658970230 ) ) ;
#20660 = CARTESIAN_POINT ( 'NONE',  ( -0.9988176903691428077, 49.83852402762217082, 93.30496380123798872 ) ) ;
#20661 = CARTESIAN_POINT ( 'NONE',  ( 4.591779561242093521, 52.09652731707507201, 76.01224951307210631 ) ) ;
#20662 = EDGE_LOOP ( 'NONE', ( #3274, #7308, #13200, #6814 ) ) ;
#20663 = EDGE_CURVE ( 'NONE', #10333, #1086, #16826, .T. ) ;
#20664 = CARTESIAN_POINT ( 'NONE',  ( -5.052695833059940078, 50.99437019215367428, 79.48628414162533318 ) ) ;
#20665 = DIRECTION ( 'NONE',  ( 0.3165065846431827645, 0.9485903129789529098, 0.000000000000000000 ) ) ;
#20666 = DIRECTION ( 'NONE',  ( 0.3165065846431827645, 0.9485903129789529098, 0.000000000000000000 ) ) ;
#20667 = CARTESIAN_POINT ( 'NONE',  ( -4.224906967831221216, 50.83896237574116839, 78.93596775356181183 ) ) ;
#20668 = EDGE_CURVE ( 'NONE', #12829, #4876, #13320, .T. ) ;
#20669 = VERTEX_POINT ( 'NONE', #18523 ) ;
#20670 = CARTESIAN_POINT ( 'NONE',  ( -5.478128554961354091, 38.57320898139802523, 75.45433879953087342 ) ) ;
#20671 = CARTESIAN_POINT ( 'NONE',  ( 0.8340537790549603647, 52.35226632664123514, 78.70464370717459701 ) ) ;
#20672 = ORIENTED_EDGE ( 'NONE', *, *, #12077, .T. ) ;
#20673 = CARTESIAN_POINT ( 'NONE',  ( -3.711822497969910817, 40.81753442731484682, 92.45433879953094447 ) ) ;
#20674 = CARTESIAN_POINT ( 'NONE',  ( 5.080276094035328427, 40.73314705485743303, 95.05433879953100984 ) ) ;
#20675 = EDGE_CURVE ( 'NONE', #7197, #16959, #16468, .T. ) ;
#20676 = AXIS2_PLACEMENT_3D ( 'NONE', #16968, #11121, #1428 ) ;
#20677 = CARTESIAN_POINT ( 'NONE',  ( -1.876873622437040590, 39.01745058958429269, 95.37621379782397923 ) ) ;
#20678 = CARTESIAN_POINT ( 'NONE',  ( 5.291217816850873668, 37.50112316868685269, 75.97264893529829521 ) ) ;
#20679 = CARTESIAN_POINT ( 'NONE',  ( 5.353448830008491477, 50.78079743354576436, 78.93442753446957738 ) ) ;
#20680 = PLANE ( 'NONE',  #78 ) ;
#20681 = ORIENTED_EDGE ( 'NONE', *, *, #3758, .F. ) ;
#20682 = CARTESIAN_POINT ( 'NONE',  ( 2.110044317469556674, 52.95423264481248538, 78.53328619179760040 ) ) ;
#20683 = CARTESIAN_POINT ( 'NONE',  ( 4.393996117251955269, 36.11308595931626542, 76.73963291717792856 ) ) ;
#20684 = ORIENTED_EDGE ( 'NONE', *, *, #10262, .T. ) ;
#20685 = DIRECTION ( 'NONE',  ( -0.9534635866061452747, -0.3015081906286225522, -2.009271279954815797E-16 ) ) ;
#20686 = CARTESIAN_POINT ( 'NONE',  ( 5.838531714063069700, 37.14529820897372758, 77.55803991379978868 ) ) ;
#20687 = CARTESIAN_POINT ( 'NONE',  ( 1.352400422481993658, 50.46853102219002096, 95.57058880123798872 ) ) ;
#20688 = DIRECTION ( 'NONE',  ( 0.007885122365275663500, 0.9999689119394085113, 1.805443505845543142E-16 ) ) ;
#20689 = ORIENTED_EDGE ( 'NONE', *, *, #9247, .F. ) ;
#20690 = AXIS2_PLACEMENT_3D ( 'NONE', #20409, #13927, #12130 ) ;
#20691 = ORIENTED_EDGE ( 'NONE', *, *, #11100, .T. ) ;
#20692 = CARTESIAN_POINT ( 'NONE',  ( -7.948187775445866521, 41.77580313715249360, 78.70894411705462801 ) ) ;
#20693 = CARTESIAN_POINT ( 'NONE',  ( 8.315010726769150651, 41.60978595976011718, 78.93540621459339945 ) ) ;
#20694 = CARTESIAN_POINT ( 'NONE',  ( 6.030184373421643151, 51.03403562479821431, 79.53335372712579954 ) ) ;
#20695 = VERTEX_POINT ( 'NONE', #18201 ) ;
#20696 = CARTESIAN_POINT ( 'NONE',  ( -4.383473025373059606, 51.47257230871590394, 78.45066232894264147 ) ) ;
#20697 = CARTESIAN_POINT ( 'NONE',  ( -7.081827087393651965, 41.08818931601138047, 79.47791035122072856 ) ) ;
#20698 = CIRCLE ( 'NONE', #12230, 3.999999999999996447 ) ;
#20699 = VECTOR ( 'NONE', #3336, 1000.000000000000114 ) ;
#20700 = ORIENTED_EDGE ( 'NONE', *, *, #1405, .F. ) ;
#20701 = CARTESIAN_POINT ( 'NONE',  ( -1.219503646467431590, 49.90383875825363447, 61.41268141275705972 ) ) ;
#20702 = CARTESIAN_POINT ( 'NONE',  ( -1.077846259693481024, 50.16218137147969713, 69.55433879953100984 ) ) ;
#20703 = CARTESIAN_POINT ( 'NONE',  ( 6.449941217757646506, 38.49637729627415439, 76.59474846278332905 ) ) ;
#20704 = EDGE_CURVE ( 'NONE', #13369, #9174, #3622, .T. ) ;
#20705 = CARTESIAN_POINT ( 'NONE',  ( 6.198496396448986090, 45.68315280215533392, 91.74246380123798872 ) ) ;
#20706 = VECTOR ( 'NONE', #12302, 1000.000000000000000 ) ;
#20707 = CARTESIAN_POINT ( 'NONE',  ( 6.443052452048888767, 38.48908422573293109, 77.56325133431154484 ) ) ;
#20708 = AXIS2_PLACEMENT_3D ( 'NONE', #16000, #19387, #1421 ) ;
#20709 = B_SPLINE_CURVE_WITH_KNOTS ( 'NONE', 3,
 ( #14893, #9709, #4889, #11410, #11623, #16407, #9810, #10127, #14587, #17880, #19573, #4995, #8526, #18097 ),
 .UNSPECIFIED., .F., .F.,
 ( 4, 2, 2, 2, 2, 2, 4 ),
 ( 0.000000000000000000, 0.0005600013223350140072, 0.0008400019835025011698, 0.001120002644669988333, 0.001400003305837475495, 0.001680003967004962441, 0.002240005289339946307 ),
 .UNSPECIFIED. ) ;
#20710 = CARTESIAN_POINT ( 'NONE',  ( -4.158578283022523081, 37.42937009194851328, 72.45433879953085921 ) ) ;
#20711 = DIRECTION ( 'NONE',  ( -0.3165065846431827645, -0.9485903129789529098, 0.000000000000000000 ) ) ;
#20712 = CARTESIAN_POINT ( 'NONE',  ( 2.522153740306505298, 47.62628298661744708, 82.55433879953099563 ) ) ;
#20713 = VECTOR ( 'NONE', #11993, 1000.000000000000114 ) ;
#20714 = ORIENTED_EDGE ( 'NONE', *, *, #6835, .F. ) ;
#20715 = DIRECTION ( 'NONE',  ( -1.402518428993831183E-16, 1.000000000000000000, -3.469446951953617147E-16 ) ) ;
#20716 = CARTESIAN_POINT ( 'NONE',  ( 8.850491666625398324, 41.31920949178531544, 79.54734031390459847 ) ) ;
#20717 = FACE_OUTER_BOUND ( 'NONE', #16202, .T. ) ;
#20718 = EDGE_LOOP ( 'NONE', ( #2611, #7078, #21025, #20593 ) ) ;
#20719 = CARTESIAN_POINT ( 'NONE',  ( -8.231989325576739347, 42.64502410771121532, 79.17794681948264213 ) ) ;
#20720 =( GEOMETRIC_REPRESENTATION_CONTEXT ( 3 ) GLOBAL_UNCERTAINTY_ASSIGNED_CONTEXT ( ( #17844 ) ) GLOBAL_UNIT_ASSIGNED_CONTEXT ( ( #1678, #12847, #17740 ) ) REPRESENTATION_CONTEXT ( 'NONE', 'WORKASPACE' ) );
#20721 = VECTOR ( 'NONE', #7576, 1000.000000000000000 ) ;
#20722 = CARTESIAN_POINT ( 'NONE',  ( 8.233139685699564225, 41.37244270010830149, 78.86985518176157939 ) ) ;
#20723 = LINE ( 'NONE', #6159, #17915 ) ;
#20724 = DIRECTION ( 'NONE',  ( -1.111814006898795283E-16, 5.922860397471810542E-17, -1.000000000000000000 ) ) ;
#20725 = DIRECTION ( 'NONE',  ( 1.540237394707284220E-16, 1.793354297423764243E-16, -1.000000000000000000 ) ) ;
#20726 = B_SPLINE_SURFACE_WITH_KNOTS ( 'NONE', 3, 1, ( 
 ( #5769, #5656 ),
 ( #18644, #876 ),
 ( #8661, #4171 ),
 ( #7361, #5882 ),
 ( #5559, #11958 ),
 ( #7037, #13537 ),
 ( #8872, #10696 ),
 ( #7256, #4060 ),
 ( #13851, #15143 ),
 ( #20332, #20008 ),
 ( #2578, #17158 ) ),
 .UNSPECIFIED., .F., .F., .F.,
 ( 4, 1, 1, 1, 1, 1, 1, 1, 4 ),
 ( 2, 2 ),
 ( 0.000000000000000000, 0.2026380577750736822, 0.3699241180509920679, 0.5036394156482512097, 0.6074627879459471025, 0.6969630674522783176, 0.7888943515530689732, 0.8885774882565341537, 1.000000000000000000 ),
 ( 0.000000000000000000, 1.000000000000000000 ),
 .UNSPECIFIED. ) ;
#20727 = CARTESIAN_POINT ( 'NONE',  ( -4.652687709939232086, 51.28020135170361016, 75.36022115247205022 ) ) ;
#20728 = CIRCLE ( 'NONE', #353, 8.199999999999995737 ) ;
#20729 = CARTESIAN_POINT ( 'NONE',  ( 8.594846595468295547, 42.91744304621954598, 77.77798975163413786 ) ) ;
#20730 = DIRECTION ( 'NONE',  ( 0.000000000000000000, -1.000000000000000000, -2.168404344970984808E-15 ) ) ;
#20731 = CARTESIAN_POINT ( 'NONE',  ( 6.961592395446249526, 50.34604203833234237, 76.59575135851817151 ) ) ;
#20732 = ORIENTED_EDGE ( 'NONE', *, *, #20903, .F. ) ;
#20733 = CARTESIAN_POINT ( 'NONE',  ( 8.787893756631273590, 41.13159958439556618, 78.49453464888588883 ) ) ;
#20734 = CARTESIAN_POINT ( 'NONE',  ( 0.5221537403065114047, 44.16218137147969713, 45.55433879953100273 ) ) ;
#20735 = EDGE_CURVE ( 'NONE', #13402, #16327, #5312, .T. ) ;
#20736 = CARTESIAN_POINT ( 'NONE',  ( -5.381123819449237899, 50.75968757759591909, 79.33884456587460932 ) ) ;
#20737 = CARTESIAN_POINT ( 'NONE',  ( 5.241460166982748525, 50.86801069014953924, 78.59183879953087626 ) ) ;
#20738 = ORIENTED_EDGE ( 'NONE', *, *, #20533, .F. ) ;
#20739 = LINE ( 'NONE', #1190, #20046 ) ;
#20740 = CARTESIAN_POINT ( 'NONE',  ( 6.102441102155617969, 43.42752260303680600, 89.86746380294499659 ) ) ;
#20741 = ORIENTED_EDGE ( 'NONE', *, *, #10377, .T. ) ;
#20742 = CARTESIAN_POINT ( 'NONE',  ( 5.535687768410739729, 50.64618487078023890, 78.75475733230618403 ) ) ;
#20743 = EDGE_CURVE ( 'NONE', #11711, #20138, #15125, .T. ) ;
#20744 = CARTESIAN_POINT ( 'NONE',  ( 3.948530577815479337, 39.69684013992245752, 94.39871379953099506 ) ) ;
#20745 = CARTESIAN_POINT ( 'NONE',  ( 9.026838159693451047, 41.84773111872319618, 78.13669174070733447 ) ) ;
#20746 = CARTESIAN_POINT ( 'NONE',  ( 11.22215374030650281, 42.76218137147968434, 77.40433879953098995 ) ) ;
#20747 = CARTESIAN_POINT ( 'NONE',  ( 0.8175694909215609485, 52.96382645516884224, 76.07424718102974737 ) ) ;
#20748 = CARTESIAN_POINT ( 'NONE',  ( -3.349688636638950889, 52.21127678364309332, 78.10580938776615767 ) ) ;
#20749 = VERTEX_POINT ( 'NONE', #13625 ) ;
#20750 = VECTOR ( 'NONE', #8858, 1000.000000000000000 ) ;
#20751 = FACE_OUTER_BOUND ( 'NONE', #13562, .T. ) ;
#20752 = ORIENTED_EDGE ( 'NONE', *, *, #15366, .F. ) ;
#20753 = CARTESIAN_POINT ( 'NONE',  ( 6.828503391016846891, 43.33193468930419101, 94.00808880123798872 ) ) ;
#20754 = CARTESIAN_POINT ( 'NONE',  ( -7.190018231056568787, 46.95048906439452452, 79.12198650143768930 ) ) ;
#20755 = CARTESIAN_POINT ( 'NONE',  ( 0.3303954077475434459, 52.35993896991258367, 76.24030295937397739 ) ) ;
#20756 = CARTESIAN_POINT ( 'NONE',  ( 5.786794573647632944, 37.10832874265046399, 76.01697444493925104 ) ) ;
#20757 = CARTESIAN_POINT ( 'NONE',  ( -7.870029994478678681, 41.50220093607910599, 78.93669174070734584 ) ) ;
#20758 = EDGE_CURVE ( 'NONE', #13884, #3900, #9180, .T. ) ;
#20759 = AXIS2_PLACEMENT_3D ( 'NONE', #18065, #13173, #19547 ) ;
#20760 = ORIENTED_EDGE ( 'NONE', *, *, #10656, .F. ) ;
#20761 = CARTESIAN_POINT ( 'NONE',  ( 4.685757199431944464, 52.02710982139440432, 77.94290914044947272 ) ) ;
#20762 = VECTOR ( 'NONE', #161, 1000.000000000000000 ) ;
#20763 = ORIENTED_EDGE ( 'NONE', *, *, #18545, .T. ) ;
#20764 = CARTESIAN_POINT ( 'NONE',  ( -2.914861642632559313, 51.60221265124933865, 76.66413924479479647 ) ) ;
#20765 = CARTESIAN_POINT ( 'NONE',  ( 4.001624342216747010, 40.29782057951908314, 90.66473080991372058 ) ) ;
#20766 = LINE ( 'NONE', #4497, #1684 ) ;
#20767 = ORIENTED_EDGE ( 'NONE', *, *, #12150, .T. ) ;
#20768 = CARTESIAN_POINT ( 'NONE',  ( -5.832343694407396306, 50.43726237516484900, 78.41225960292398156 ) ) ;
#20769 = CARTESIAN_POINT ( 'NONE',  ( -5.121096889713498079, 43.19689566777418577, 95.05433879953096721 ) ) ;
#20770 = ORIENTED_EDGE ( 'NONE', *, *, #3774, .F. ) ;
#20771 = CARTESIAN_POINT ( 'NONE',  ( 6.830172062167755520, 37.85388809545894873, 77.80469260682309596 ) ) ;
#20772 = EDGE_CURVE ( 'NONE', #19214, #1174, #17139, .T. ) ;
#20773 = CARTESIAN_POINT ( 'NONE',  ( -4.414789981656704221, 51.45019435834255717, 78.82303764823565473 ) ) ;
#20774 = EDGE_LOOP ( 'NONE', ( #19074, #3184, #20630, #14260, #4625 ) ) ;
#20775 = CARTESIAN_POINT ( 'NONE',  ( -4.337338579526520910, 46.33133051644502132, 92.55433879953099563 ) ) ;
#20776 = CARTESIAN_POINT ( 'NONE',  ( 5.611423337425062385, 41.22389019960463230, 92.83621380123797451 ) ) ;
#20777 = ADVANCED_FACE ( 'NONE', ( #1180 ), #14047, .F. ) ;
#20778 = VECTOR ( 'NONE', #15473, 1000.000000000000227 ) ;
#20779 = ORIENTED_EDGE ( 'NONE', *, *, #9272, .T. ) ;
#20780 = CARTESIAN_POINT ( 'NONE',  ( 4.609531566588798590, 52.08341462581984871, 78.11943565213420015 ) ) ;
#20781 = DIRECTION ( 'NONE',  ( 0.9534635866061451637, 0.3015081906286225522, 2.009271279954815797E-16 ) ) ;
#20782 = CARTESIAN_POINT ( 'NONE',  ( -5.319578332459784065, 49.88389014699610868, 75.98690818113186651 ) ) ;
#20783 = CARTESIAN_POINT ( 'NONE',  ( 2.635245049009970142, 48.69372030666295359, 91.39183879611699979 ) ) ;
#20784 = CARTESIAN_POINT ( 'NONE',  ( 5.078529275337140270, 37.34914372394564452, 76.44059830477070250 ) ) ;
#20785 = EDGE_CURVE ( 'NONE', #5209, #10061, #4502, .T. ) ;
#20787 = EDGE_CURVE ( 'NONE', #19686, #15280, #2663, .T. ) ;
#20786 = LINE ( 'NONE', #14310, #5405 ) ;
#20788 = ADVANCED_FACE ( 'NONE', ( #9058 ), #17353, .T. ) ;
#20789 = CARTESIAN_POINT ( 'NONE',  ( 5.528499006811445682, 50.64997445399101395, 76.04053158567903381 ) ) ;
#20790 = ADVANCED_FACE ( 'NONE', ( #4350 ), #2775, .T. ) ;
#20791 = ORIENTED_EDGE ( 'NONE', *, *, #2874, .F. ) ;
#20792 = CARTESIAN_POINT ( 'NONE',  ( 1.580015341223601766, 52.89863773268244529, 76.85864713079314470 ) ) ;
#20793 = DIRECTION ( 'NONE',  ( -0.5813877811927011807, 0.8136266022444372803, 5.636455622144619183E-17 ) ) ;
#20794 = ORIENTED_EDGE ( 'NONE', *, *, #15109, .T. ) ;
#20795 = AXIS2_PLACEMENT_3D ( 'NONE', #2223, #617, #2324 ) ;
#20796 = LINE ( 'NONE', #1343, #12246 ) ;
#20797 = ADVANCED_FACE ( 'NONE', ( #5858 ), #14801, .T. ) ;
#20798 = CARTESIAN_POINT ( 'NONE',  ( 5.847824973458005005, 37.15193883188941015, 77.47236191065434241 ) ) ;
#20799 = DIRECTION ( 'NONE',  ( -0.000000000000000000, -0.000000000000000000, 1.000000000000000000 ) ) ;
#20800 = VECTOR ( 'NONE', #17906, 1000.000000000000000 ) ;
#20801 = LINE ( 'NONE', #8043, #10523 ) ;
#20802 = VERTEX_POINT ( 'NONE', #7982 ) ;
#20803 = CARTESIAN_POINT ( 'NONE',  ( 26.43948732994507367, 43.16218137147969003, 74.70433879953098710 ) ) ;
#20804 = CARTESIAN_POINT ( 'NONE',  ( -3.373121299339454815, 37.02388247401010091, 75.61442449207443417 ) ) ;
#20805 = DIRECTION ( 'NONE',  ( 0.7071067811865506814, -0.7071067811865443531, 0.000000000000000000 ) ) ;
#20806 = CARTESIAN_POINT ( 'NONE',  ( -5.334571511159140300, 49.90167720919038175, 75.98434391831075629 ) ) ;
#20807 = ORIENTED_EDGE ( 'NONE', *, *, #8726, .F. ) ;
#20808 = CARTESIAN_POINT ( 'NONE',  ( 24.43948732994508077, 43.16218137147968292, 76.90433879953101837 ) ) ;
#20809 = CARTESIAN_POINT ( 'NONE',  ( -5.130197398460217606, 37.39693086210134254, 77.90166954077812989 ) ) ;
#20810 = CARTESIAN_POINT ( 'NONE',  ( 0.2860873169776696479, 38.75537135769874197, 94.90746379953098710 ) ) ;
#20811 = VERTEX_POINT ( 'NONE', #14363 ) ;
#20812 = LINE ( 'NONE', #17942, #13135 ) ;
#20813 = CARTESIAN_POINT ( 'NONE',  ( -6.824509517481986087, 40.67530721073914179, 79.25635544885822981 ) ) ;
#20814 = CARTESIAN_POINT ( 'NONE',  ( 6.449077564475651059, 38.49547022419763920, 76.49624899266501643 ) ) ;
#20815 = CARTESIAN_POINT ( 'NONE',  ( 1.352400422481993658, 50.46853102219002096, 93.22683880123798872 ) ) ;
#20816 = CIRCLE ( 'NONE', #7912, 1.399999999999995026 ) ;
#20817 =( NAMED_UNIT ( * ) SI_UNIT ( $, .STERADIAN. ) SOLID_ANGLE_UNIT ( ) );
#20818 = CARTESIAN_POINT ( 'NONE',  ( -4.790713360849209401, 51.18157327500495768, 75.36324311589748959 ) ) ;
#20819 = CARTESIAN_POINT ( 'NONE',  ( 5.396517835962451493, 50.75616155517602834, 78.93669174070734584 ) ) ;
#20820 = EDGE_CURVE ( 'NONE', #271, #20036, #12979, .T. ) ;
#20821 = DIRECTION ( 'NONE',  ( 1.540237394707284220E-16, 1.793354297423764243E-16, -1.000000000000000000 ) ) ;
#20822 = CARTESIAN_POINT ( 'NONE',  ( -0.8946779508733179176, 52.21709741114992909, 78.78847851419276083 ) ) ;
#20823 = CARTESIAN_POINT ( 'NONE',  ( 31.22215374030650281, 42.76218137147968434, 78.80433879953099563 ) ) ;
#20824 = LINE ( 'NONE', #6152, #8219 ) ;
#20825 = EDGE_CURVE ( 'NONE', #10505, #13618, #11580, .T. ) ;
#20826 = CARTESIAN_POINT ( 'NONE',  ( 8.744145067270602922, 41.00048198701652780, 79.52393066155629242 ) ) ;
#20827 = CARTESIAN_POINT ( 'NONE',  ( 5.389492195292208798, 36.82443100924615464, 78.09625056423675460 ) ) ;
#20828 = ORIENTED_EDGE ( 'NONE', *, *, #8390, .F. ) ;
#20829 = CIRCLE ( 'NONE', #105, 4.200000000000001954 ) ;
#20830 = VERTEX_POINT ( 'NONE', #12669 ) ;
#20831 = CARTESIAN_POINT ( 'NONE',  ( 8.263416355632948296, 41.45783420393981089, 78.92242849838478946 ) ) ;
#20832 = CARTESIAN_POINT ( 'NONE',  ( -4.323846805489818479, 36.80131216085734991, 79.51042285023450518 ) ) ;
#20833 = CARTESIAN_POINT ( 'NONE',  ( 0.5221537403065064087, 48.16218137147969003, 46.35433879953098568 ) ) ;
#20834 = ADVANCED_FACE ( 'NONE', ( #11289 ), #5287, .T. ) ;
#20835 = CARTESIAN_POINT ( 'NONE',  ( 27.03948732994508219, 43.16218137147969003, 75.00433879953099847 ) ) ;
#20836 = CARTESIAN_POINT ( 'NONE',  ( 5.287808634542578545, 50.82928320178807269, 77.98642840401727483 ) ) ;
#20837 = CARTESIAN_POINT ( 'NONE',  ( 6.616107328214575034, 50.60123794050897317, 77.65065976741861675 ) ) ;
#20838 = FACE_OUTER_BOUND ( 'NONE', #6727, .T. ) ;
#20839 =( BOUNDED_CURVE ( )  B_SPLINE_CURVE ( 2, ( #12170, #20338, #12282, #18762, #15151 ),
 .UNSPECIFIED., .F., .F. ) 
 B_SPLINE_CURVE_WITH_KNOTS ( ( 3, 2, 3 ),
 ( 0.8923390146554854852, 0.9062500000000000000, 0.9200238926711118426 ),
 .UNSPECIFIED. ) 
 CURVE ( )  GEOMETRIC_REPRESENTATION_ITEM ( )  RATIONAL_B_SPLINE_CURVE ( ( 0.9623977609649205789, 0.9661148573551012753, 1.000000000000000000, 0.9664487952235394363, 0.9624739548360365937 ) ) 
 REPRESENTATION_ITEM ( '' )  );
#20840 = VECTOR ( 'NONE', #5187, 1000.000000000000114 ) ;
#20841 = ORIENTED_EDGE ( 'NONE', *, *, #1848, .F. ) ;
#20842 = CARTESIAN_POINT ( 'NONE',  ( -4.412207535196425390, 37.80258716859745505, 79.54807357191100436 ) ) ;
#20843 = DIRECTION ( 'NONE',  ( -1.540237394707284467E-16, -1.793354297423764243E-16, 1.000000000000000000 ) ) ;
#20844 = LINE ( 'NONE', #9487, #6163 ) ;
#20845 = VERTEX_POINT ( 'NONE', #2219 ) ;
#20846 = PLANE ( 'NONE',  #15996 ) ;
#20847 = CARTESIAN_POINT ( 'NONE',  ( -4.500660556396669065, 42.81632233694663370, 90.57058880294496817 ) ) ;
#20848 = ORIENTED_EDGE ( 'NONE', *, *, #4294, .T. ) ;
#20849 = CARTESIAN_POINT ( 'NONE',  ( -0.9296126965184758895, 52.21939493466130955, 76.40919915166844589 ) ) ;
#20850 = CARTESIAN_POINT ( 'NONE',  ( 4.905034931190686009, 51.86513819399005598, 79.33697856897433098 ) ) ;
#20851 = CARTESIAN_POINT ( 'NONE',  ( 5.577191696014057953, 37.87832978262304096, 78.37198585835440667 ) ) ;
#20852 =( NAMED_UNIT ( * ) SI_UNIT ( $, .STERADIAN. ) SOLID_ANGLE_UNIT ( ) );
#20853 = CARTESIAN_POINT ( 'NONE',  ( 3.889041150776882727, 48.17793082961422613, 92.45433879953097289 ) ) ;
#20854 = EDGE_LOOP ( 'NONE', ( #2154, #17081, #6719, #12900 ) ) ;
#20855 = CARTESIAN_POINT ( 'NONE',  ( 31.22215374030650281, 42.96218137147968008, 77.80433879953099563 ) ) ;
#20856 = ORIENTED_EDGE ( 'NONE', *, *, #13855, .F. ) ;
#20857 = DIRECTION ( 'NONE',  ( 0.5813877811926937422, -0.8136266022444427204, -5.636455622144829957E-17 ) ) ;
#20858 = DIRECTION ( 'NONE',  ( 1.000000000000000000, -0.000000000000000000, -0.000000000000000000 ) ) ;
#20859 = CARTESIAN_POINT ( 'NONE',  ( -7.583764859133458991, 47.59007672682779599, 78.90843038313050783 ) ) ;
#20860 = CARTESIAN_POINT ( 'NONE',  ( 5.848563030374239524, 37.15246622033975399, 76.55482881315118959 ) ) ;
#20861 = DIRECTION ( 'NONE',  ( 3.154042683594179442E-15, 0.000000000000000000, -1.000000000000000000 ) ) ;
#20862 = ORIENTED_EDGE ( 'NONE', *, *, #19087, .T. ) ;
#20863 = CARTESIAN_POINT ( 'NONE',  ( 8.220041259636596820, 41.33680711362989513, 76.16501461267081652 ) ) ;
#20864 = ORIENTED_EDGE ( 'NONE', *, *, #1337, .F. ) ;
#20865 = CARTESIAN_POINT ( 'NONE',  ( -4.004103039135145536, 51.74365621125981107, 75.44813358671753178 ) ) ;
#20866 = CARTESIAN_POINT ( 'NONE',  ( -4.524181921268124462, 40.28999182795290324, 94.94558880123797451 ) ) ;
#20867 = CARTESIAN_POINT ( 'NONE',  ( -7.854651159657231041, 41.44641869631179532, 78.04033446252860529 ) ) ;
#20868 = VERTEX_POINT ( 'NONE', #8508 ) ;
#20869 = CARTESIAN_POINT ( 'NONE',  ( 2.113288515708719117, 52.20632789671663687, 77.70145201013903602 ) ) ;
#20870 = LINE ( 'NONE', #17282, #8250 ) ;
#20871 = CARTESIAN_POINT ( 'NONE',  ( 6.604417847172709521, 37.69257239881283539, 78.19824744938543404 ) ) ;
#20872 = CARTESIAN_POINT ( 'NONE',  ( -1.218186307993342599, 38.53589529967370453, 95.05433879953095300 ) ) ;
#20873 = EDGE_CURVE ( 'NONE', #2188, #7787, #6681, .T. ) ;
#20874 = CARTESIAN_POINT ( 'NONE',  ( 5.113845713194847598, 37.37437955742144879, 77.68578589458712713 ) ) ;
#20875 = ORIENTED_EDGE ( 'NONE', *, *, #8807, .F. ) ;
#20876 = CARTESIAN_POINT ( 'NONE',  ( 6.433553176315260913, 38.47928099333162777, 72.45433879953087342 ) ) ;
#20877 = CARTESIAN_POINT ( 'NONE',  ( 31.07218010054375412, 42.96218137147968008, 66.20574467885104752 ) ) ;
#20878 = ORIENTED_EDGE ( 'NONE', *, *, #3001, .T. ) ;
#20879 = CARTESIAN_POINT ( 'NONE',  ( 5.008975552073979820, 51.78836144432717248, 77.68963291717793140 ) ) ;
#20880 = CARTESIAN_POINT ( 'NONE',  ( 5.420351613492021770, 41.31768866812478080, 95.05433879953098142 ) ) ;
#20881 = CARTESIAN_POINT ( 'NONE',  ( 2.522153740306498193, 49.81903562097208038, 123.5543387995310098 ) ) ;
#20882 = CARTESIAN_POINT ( 'NONE',  ( 2.463659247115867590, 38.82793883177424732, 91.78246379782397923 ) ) ;
#20883 = CARTESIAN_POINT ( 'NONE',  ( 28.52215374030649642, 44.16218137147969003, 87.85433879953103542 ) ) ;
#20884 = CARTESIAN_POINT ( 'NONE',  ( 11.22215374030649926, 48.36218137147968577, 80.55433879953099563 ) ) ;
#20885 = ADVANCED_FACE ( 'NONE', ( #5514 ), #11915, .F. ) ;
#20886 = VERTEX_POINT ( 'NONE', #20078 ) ;
#20887 = CARTESIAN_POINT ( 'NONE',  ( 2.114902586664012318, 52.20151937974352307, 78.20017459567505114 ) ) ;
#20888 = ORIENTED_EDGE ( 'NONE', *, *, #8534, .F. ) ;
#20889 = CARTESIAN_POINT ( 'NONE',  ( -5.661408436751226070, 39.74363423441516829, 75.45433879953087342 ) ) ;
#20890 = CARTESIAN_POINT ( 'NONE',  ( -0.8635238853855432550, 52.24432082531686916, 76.01832139834691304 ) ) ;
#20891 = CARTESIAN_POINT ( 'NONE',  ( 9.122633311574107395, 42.13483526604063201, 79.44701590970058191 ) ) ;
#20892 = EDGE_CURVE ( 'NONE', #5204, #899, #13493, .T. ) ;
#20893 = B_SPLINE_SURFACE_WITH_KNOTS ( 'NONE', 3, 1, ( 
 ( #4397, #10921 ),
 ( #11023, #20667 ),
 ( #19287, #4700 ),
 ( #8017, #17391 ),
 ( #15808, #17494 ),
 ( #2918, #17699 ),
 ( #20773, #6208 ),
 ( #12707, #19186 ),
 ( #13337, #14817 ),
 ( #18123, #3328 ),
 ( #18222, #1638 ),
 ( #236, #3543 ),
 ( #10047, #5019 ),
 ( #14718, #4912 ),
 ( #18013, #8120 ) ),
 .UNSPECIFIED., .F., .F., .F.,
 ( 4, 1, 1, 1, 1, 1, 1, 1, 1, 1, 1, 1, 4 ),
 ( 2, 2 ),
 ( 0.000000000000000000, 0.1142047618744220089, 0.2098279651953024738, 0.2930641324527410441, 0.3714084400245239448, 0.4142179382887971051, 0.4671782061414135323, 0.5290873093409070860, 0.6015893617863945497, 0.6852532414128420513, 0.7789222961280750646, 0.8837899115430479791, 1.000000000000000000 ),
 ( 0.000000000000000000, 1.000000000000000000 ),
 .UNSPECIFIED. ) ;
#20894 = FACE_OUTER_BOUND ( 'NONE', #4429, .T. ) ;
#20895 = ORIENTED_EDGE ( 'NONE', *, *, #1413, .T. ) ;
#20896 = CARTESIAN_POINT ( 'NONE',  ( 5.611423337425062385, 41.22389019960463230, 94.08621380123797451 ) ) ;
#20897 = ORIENTED_EDGE ( 'NONE', *, *, #1191, .F. ) ;
#20898 = CARTESIAN_POINT ( 'NONE',  ( -4.509672285278094606, 36.93857395727002313, 75.36838243422435824 ) ) ;
#20899 = FACE_OUTER_BOUND ( 'NONE', #14073, .T. ) ;
#20900 = CARTESIAN_POINT ( 'NONE',  ( 4.987494971863720927, 47.58855820898865829, 93.46121379953098085 ) ) ;
#20901 = VERTEX_POINT ( 'NONE', #15201 ) ;
#20902 = CARTESIAN_POINT ( 'NONE',  ( -4.641234702847274463, 37.03575381547093315, 77.24798498253255730 ) ) ;
#20903 = EDGE_CURVE ( 'NONE', #9268, #17689, #411, .T. ) ;
#20904 = FACE_OUTER_BOUND ( 'NONE', #169, .T. ) ;
#20905 = CARTESIAN_POINT ( 'NONE',  ( 4.178421596892071044, 40.17206517740157778, 92.56371379953098710 ) ) ;
#20906 = ORIENTED_EDGE ( 'NONE', *, *, #5472, .F. ) ;
#20907 = CARTESIAN_POINT ( 'NONE',  ( -4.804273704418943858, 51.17188354996588373, 76.37148643835737971 ) ) ;
#20908 = PRESENTATION_STYLE_ASSIGNMENT (( #3058 ) ) ;
#20909 = DIRECTION ( 'NONE',  ( -0.5941461771851693774, -0.8043570849667760481, -2.357623395011396791E-16 ) ) ;
#20910 = CARTESIAN_POINT ( 'NONE',  ( 1.352400422481993658, 50.46853102219002096, 91.97683880123797451 ) ) ;
#20911 = EDGE_CURVE ( 'NONE', #9681, #3376, #16486, .T. ) ;
#20912 = CARTESIAN_POINT ( 'NONE',  ( 4.987494971863720927, 47.58855820898865829, 90.02371380294498238 ) ) ;
#20913 = CARTESIAN_POINT ( 'NONE',  ( 8.806278593017598411, 41.18670010535765869, 77.44807837618913027 ) ) ;
#20914 = LINE ( 'NONE', #12750, #13569 ) ;
#20915 = CARTESIAN_POINT ( 'NONE',  ( -0.9364695654124475244, 52.21742695338924278, 78.32762347114741885 ) ) ;
#20916 = ORIENTED_EDGE ( 'NONE', *, *, #20131, .T. ) ;
#20917 = CARTESIAN_POINT ( 'NONE',  ( 6.635267586053947397, 39.64667042487232607, 75.45433879953087342 ) ) ;
#20918 = DIRECTION ( 'NONE',  ( -1.402518428993831676E-16, 1.000000000000000000, 0.000000000000000000 ) ) ;
#20919 = CARTESIAN_POINT ( 'NONE',  ( 0.8269786168830152162, 52.35651847692464855, 76.08306728897994731 ) ) ;
#20920 = CARTESIAN_POINT ( 'NONE',  ( 5.902048492000326441, 51.12868443877599134, 78.59183879953087626 ) ) ;
#20921 = VERTEX_POINT ( 'NONE', #19967 ) ;
#20922 = AXIS2_PLACEMENT_3D ( 'NONE', #17757, #6573, #9690 ) ;
#20923 = EDGE_CURVE ( 'NONE', #8675, #8877, #16590, .T. ) ;
#20924 = CARTESIAN_POINT ( 'NONE',  ( 9.350741246242593618, 42.81848921713964984, 76.37534566197098229 ) ) ;
#20926 = ADVANCED_FACE ( 'NONE', ( #13600 ), #2010, .F. ) ;
#20925 = DIRECTION ( 'NONE',  ( -1.110223024625156540E-16, -1.000000000000000000, -5.922860397471808077E-17 ) ) ;
#20927 = CARTESIAN_POINT ( 'NONE',  ( -4.893796645199858020, 37.22231114847116373, 78.64904841171450300 ) ) ;
#20928 = CARTESIAN_POINT ( 'NONE',  ( -4.453436368711327198, 50.68011839687689957, 72.45433879953087342 ) ) ;
#20929 = CARTESIAN_POINT ( 'NONE',  ( 0.5221537403065064087, 48.16218137147969003, 53.55433879953100273 ) ) ;
#20930 = CARTESIAN_POINT ( 'NONE',  ( -3.287686668943208268, 36.90074446973970623, 75.72657343730216439 ) ) ;
#20931 = CARTESIAN_POINT ( 'NONE',  ( 6.961907239250668233, 50.34580947589670075, 76.63889762306028786 ) ) ;
#20932 = CARTESIAN_POINT ( 'NONE',  ( -1.219056181836354558, 49.77488197367695477, 94.40612966814926210 ) ) ;
#20933 = CARTESIAN_POINT ( 'NONE',  ( 5.202885763635528349, 50.89499265101085967, 76.39036821129558064 ) ) ;
#20934 = EDGE_CURVE ( 'NONE', #5980, #11406, #14964, .T. ) ;
#20935 = ADVANCED_FACE ( 'NONE', ( #18280 ), #13400, .F. ) ;
#20936 = AXIS2_PLACEMENT_3D ( 'NONE', #15365, #17163, #2585 ) ;
#20937 = CARTESIAN_POINT ( 'NONE',  ( -5.606854386412799762, 37.74901817818727778, 79.39214668191834789 ) ) ;
#20938 = ADVANCED_FACE ( 'NONE', ( #16697 ), #17041, .T. ) ;
#20939 = CARTESIAN_POINT ( 'NONE',  ( -5.616859571223690395, 50.59123944021462904, 79.13778479689705136 ) ) ;
#20940 = CARTESIAN_POINT ( 'NONE',  ( 5.246091170965059725, 50.86474954119325531, 78.73919069833695517 ) ) ;
#20941 = FACE_OUTER_BOUND ( 'NONE', #17011, .T. ) ;
#20942 = CARTESIAN_POINT ( 'NONE',  ( 9.106328434870372135, 42.08596851619746104, 78.11626675975762168 ) ) ;
#20943 = EDGE_LOOP ( 'NONE', ( #13768, #16178, #1711, #18377 ) ) ;
#20944 = CARTESIAN_POINT ( 'NONE',  ( 6.721999984869559519, 37.77659228945417880, 75.79056106475293575 ) ) ;
#20945 = AXIS2_PLACEMENT_3D ( 'NONE', #2557, #10560, #9053 ) ;
#20946 = DIRECTION ( 'NONE',  ( -0.5941461771851693774, -0.8043570849667760481, -2.357623395011396791E-16 ) ) ;
#20947 = CARTESIAN_POINT ( 'NONE',  ( 7.688394307443750186, 40.17658030797320379, 78.53633816310291138 ) ) ;
#20948 = FILL_AREA_STYLE ('',( #9188 ) ) ;
#20949 = CARTESIAN_POINT ( 'NONE',  ( 5.269956278383879145, 45.96059190786396442, 92.45433879953094447 ) ) ;
#20950 = ORIENTED_EDGE ( 'NONE', *, *, #15594, .F. ) ;
#20951 =( BOUNDED_CURVE ( )  B_SPLINE_CURVE ( 3, ( #10644, #4222, #12643, #20701 ),
 .UNSPECIFIED., .F., .F. ) 
 B_SPLINE_CURVE_WITH_KNOTS ( ( 4, 4 ),
 ( 1.230959417340772521, 1.276280841686757039 ),
 .UNSPECIFIED. ) 
 CURVE ( )  GEOMETRIC_REPRESENTATION_ITEM ( )  RATIONAL_B_SPLINE_CURVE ( ( 1.000000000000000000, 0.9998288380325438540, 0.9998288380325438540, 1.000000000000000000 ) ) 
 REPRESENTATION_ITEM ( '' )  );
#20952 = CARTESIAN_POINT ( 'NONE',  ( 8.364438980634542276, 41.78253443625140306, 76.11674899411023887 ) ) ;
#20953 = ORIENTED_EDGE ( 'NONE', *, *, #6660, .F. ) ;
#20954 = CARTESIAN_POINT ( 'NONE',  ( -2.416137431568557314, 39.07291177436112406, 94.86746380123797451 ) ) ;
#20955 = EDGE_CURVE ( 'NONE', #2109, #13986, #7537, .T. ) ;
#20956 = CARTESIAN_POINT ( 'NONE',  ( 2.043125170982144745, 38.48583871533720213, 92.52371380123798872 ) ) ;
#20957 = CARTESIAN_POINT ( 'NONE',  ( -7.830524803375885412, 46.93262048933035402, 79.27433398498862971 ) ) ;
#20958 = LINE ( 'NONE', #15992, #19488 ) ;
#20959 = PLANE ( 'NONE',  #4470 ) ;
#20960 = VECTOR ( 'NONE', #653, 1000.000000000000000 ) ;
#20961 = EDGE_LOOP ( 'NONE', ( #9543, #20597, #15608, #13222, #5021, #927 ) ) ;
#20962 = CARTESIAN_POINT ( 'NONE',  ( 0.5221537403065019678, 44.16218137147968292, 72.45433879953087342 ) ) ;
#20963 = ORIENTED_EDGE ( 'NONE', *, *, #16366, .F. ) ;
#20964 = FACE_OUTER_BOUND ( 'NONE', #12205, .T. ) ;
#20965 = CARTESIAN_POINT ( 'NONE',  ( -0.3080929418689875576, 37.85583172076933778, 91.35183880123798872 ) ) ;
#20966 = CARTESIAN_POINT ( 'NONE',  ( 2.043125170982144745, 38.48583871533720213, 95.02371380123798872 ) ) ;
#20967 = EDGE_LOOP ( 'NONE', ( #20030, #12152 ) ) ;
#20968 = CARTESIAN_POINT ( 'NONE',  ( 1.825099168086168122, 52.25818555367717266, 76.99764931820573111 ) ) ;
#20969 = CARTESIAN_POINT ( 'NONE',  ( -5.940171601930140710, 37.99522617845349970, 78.80728580974474085 ) ) ;
#20970 = AXIS2_PLACEMENT_3D ( 'NONE', #2491, #561, #4179 ) ;
#20971 = CARTESIAN_POINT ( 'NONE',  ( 5.504730982882359847, 46.12534449621361432, 92.55433879953100984 ) ) ;
#20972 = DIRECTION ( 'NONE',  ( -3.893792155548169402E-16, -7.183611964723547524E-17, 1.000000000000000000 ) ) ;
#20973 = DIRECTION ( 'NONE',  ( 0.3165065846431826535, 0.9485903129789529098, 2.188653791613874008E-16 ) ) ;
#20974 = EDGE_LOOP ( 'NONE', ( #14984, #6257, #19852, #8707 ) ) ;
#20975 = CARTESIAN_POINT ( 'NONE',  ( 0.5221537403065006355, 44.16218137147969003, 92.45433879953097289 ) ) ;
#20976 = CARTESIAN_POINT ( 'NONE',  ( 23.63948732994508717, 43.16218137147969003, 74.70433879953098710 ) ) ;
#20977 = VERTEX_POINT ( 'NONE', #20608 ) ;
#20978 = CARTESIAN_POINT ( 'NONE',  ( 0.2343434307403843286, 49.48026920881595458, 95.05433879953099563 ) ) ;
#20979 = DIRECTION ( 'NONE',  ( -0.3165065846431828200, -0.9485903129789529098, 0.000000000000000000 ) ) ;
#20980 = CARTESIAN_POINT ( 'NONE',  ( -5.818890812078571173, 50.44687531233557110, 76.28720437108826502 ) ) ;
#20981 = CARTESIAN_POINT ( 'NONE',  ( -3.467962453771612275, 40.50591351489412517, 94.43871379611699979 ) ) ;
#20982 = CARTESIAN_POINT ( 'NONE',  ( 5.666884522201895535, 41.76315400873614436, 93.03246379782397923 ) ) ;
#20983 = DIRECTION ( 'NONE',  ( -9.598494438985368964E-18, 5.922860397471809309E-17, -1.000000000000000000 ) ) ;
#20984 = DIRECTION ( 'NONE',  ( -1.000000000000000000, -5.084437235940625660E-16, 0.000000000000000000 ) ) ;
#20985 = CIRCLE ( 'NONE', #6739, 4.200000000000003730 ) ;
#20986 = CARTESIAN_POINT ( 'NONE',  ( -3.495943983152256518, 36.18977369595653215, 76.77671532909576513 ) ) ;
#20987 = ORIENTED_EDGE ( 'NONE', *, *, #7405, .F. ) ;
#20988 = CARTESIAN_POINT ( 'NONE',  ( 2.120940930817759362, 52.95414672101166076, 78.16610350541323271 ) ) ;
#20989 = EDGE_CURVE ( 'NONE', #1059, #15210, #2751, .T. ) ;
#20990 = CARTESIAN_POINT ( 'NONE',  ( -3.623336461783060791, 52.01573806668144329, 75.70044805065693083 ) ) ;
#20991 = VERTEX_POINT ( 'NONE', #12120 ) ;
#20992 = LINE ( 'NONE', #19110, #5779 ) ;
#20993 = LINE ( 'NONE', #16549, #20439 ) ;
#20994 = CARTESIAN_POINT ( 'NONE',  ( 9.223886884231923489, 42.43829864670298946, 79.29919401074631935 ) ) ;
#20995 = FACE_OUTER_BOUND ( 'NONE', #5278, .T. ) ;
#20996 = ORIENTED_EDGE ( 'NONE', *, *, #6765, .T. ) ;
#20997 = DIRECTION ( 'NONE',  ( 1.540237394707284220E-16, 1.793354297423764243E-16, -1.000000000000000000 ) ) ;
#20998 = ORIENTED_EDGE ( 'NONE', *, *, #8088, .T. ) ;
#20999 = CARTESIAN_POINT ( 'NONE',  ( -3.777846259693486974, 51.36218137147968577, 93.55433879953098142 ) ) ;
#21000 = CARTESIAN_POINT ( 'NONE',  ( -0.9199438314403610706, 52.23437776363726215, 72.45433879953087342 ) ) ;
#21001 = CARTESIAN_POINT ( 'NONE',  ( -4.500660556396669065, 42.81632233694663370, 95.25808879953098085 ) ) ;
#21002 = ORIENTED_EDGE ( 'NONE', *, *, #14059, .F. ) ;
#21003 = DIRECTION ( 'NONE',  ( -0.3165065846431827645, -0.9485903129789529098, 0.000000000000000000 ) ) ;
#21004 = CARTESIAN_POINT ( 'NONE',  ( 8.229810522273906415, 41.37904440587443844, 77.44807837618913027 ) ) ;
#21005 = CARTESIAN_POINT ( 'NONE',  ( -3.134114116279072881, 48.15229756555780227, 93.18871379953097289 ) ) ;
#21006 = EDGE_CURVE ( 'NONE', #16680, #9248, #8368, .T. ) ;
#21007 = AXIS2_PLACEMENT_3D ( 'NONE', #17997, #19580, #9402 ) ;
#21008 = ORIENTED_EDGE ( 'NONE', *, *, #5900, .T. ) ;
#21009 = CARTESIAN_POINT ( 'NONE',  ( 0.8377421044266867289, 51.35991668224300355, 78.52566232894263010 ) ) ;
#21010 = DIRECTION ( 'NONE',  ( 0.009567942452863074584, -0.9999542261909885044, -1.778535306010356147E-16 ) ) ;
#21011 = CARTESIAN_POINT ( 'NONE',  ( 5.853714975924201980, 37.93131711438793729, 75.43046809281631226 ) ) ;
#21012 = UNCERTAINTY_MEASURE_WITH_UNIT (LENGTH_MEASURE( 1.000000000000000082E-05 ), #1255, 'distance_accuracy_value', 'NONE');
#21013 = CARTESIAN_POINT ( 'NONE',  ( 2.043125170982144745, 38.48583871533720213, 92.52371380123798872 ) ) ;
#21014 = CARTESIAN_POINT ( 'NONE',  ( -5.283659240720997019, 50.82933219714914230, 75.48294376282896678 ) ) ;
#21015 = CARTESIAN_POINT ( 'NONE',  ( 6.691294758883309157, 37.75465145915448062, 78.79551527011911105 ) ) ;
#21016 = CARTESIAN_POINT ( 'NONE',  ( 1.087883311600626124, 52.96210244217081708, 76.77198585835439815 ) ) ;
#21017 = DIRECTION ( 'NONE',  ( 0.3165065846431826535, 0.9485903129789529098, 2.188653791613874008E-16 ) ) ;
#21018 = AXIS2_PLACEMENT_3D ( 'NONE', #5333, #15035, #13122 ) ;
#21019 = CARTESIAN_POINT ( 'NONE',  ( -0.8508103573721612634, 52.21675149905355795, 78.90127229107831397 ) ) ;
#21020 = ORIENTED_EDGE ( 'NONE', *, *, #14455, .F. ) ;
#21021 = CARTESIAN_POINT ( 'NONE',  ( -3.566438244846302119, 38.23101125920473464, 78.34992703482498655 ) ) ;
#21022 = CARTESIAN_POINT ( 'NONE',  ( 9.350741246242593618, 42.81848921713964984, 76.37534566197098229 ) ) ;
#21023 = FACE_OUTER_BOUND ( 'NONE', #9452, .T. ) ;
#21024 = FACE_OUTER_BOUND ( 'NONE', #15938, .T. ) ;
#21025 = ORIENTED_EDGE ( 'NONE', *, *, #14769, .F. ) ;
#21026 = AXIS2_PLACEMENT_3D ( 'NONE', #18699, #10528, #15732 ) ;
#21027 = ORIENTED_EDGE ( 'NONE', *, *, #12500, .F. ) ;
#21028 = AXIS2_PLACEMENT_3D ( 'NONE', #15593, #17084, #1008 ) ;
#21029 = ADVANCED_FACE ( 'NONE', ( #9254 ), #2436, .T. ) ;
#21030 = CARTESIAN_POINT ( 'NONE',  ( 7.787730317602713725, 40.36046389751859209, 75.80943290476855623 ) ) ;
#21031 = CARTESIAN_POINT ( 'NONE',  ( 6.545534159973747990, 50.65336749702785113, 77.68963291717794561 ) ) ;
#21032 = CARTESIAN_POINT ( 'NONE',  ( -1.477846259693492481, 50.16218137147969713, 66.55433879953099563 ) ) ;
#21033 = CARTESIAN_POINT ( 'NONE',  ( 0.3653115025297660190, 52.36068438868553443, 78.81268202337827233 ) ) ;
#21034 = EDGE_CURVE ( 'NONE', #1640, #19441, #15741, .T. ) ;
#21035 = NEXT_ASSEMBLY_USAGE_OCCURRENCE ( 'NAUO1', ' ', ' ', #385, #11075, $ ) ;
#21036 = NEXT_ASSEMBLY_USAGE_OCCURRENCE ( 'NAUO2', ' ', ' ', #385, #8857, $ ) ;
#21037 = NEXT_ASSEMBLY_USAGE_OCCURRENCE ( 'NAUO3', ' ', ' ', #385, #16133, $ ) ;
#21038 = NEXT_ASSEMBLY_USAGE_OCCURRENCE ( 'NAUO4', ' ', ' ', #385, #8194, $ ) ;
#21039 = NEXT_ASSEMBLY_USAGE_OCCURRENCE ( 'NAUO5', ' ', ' ', #385, #14822, $ ) ;
#21040 = NEXT_ASSEMBLY_USAGE_OCCURRENCE ( 'NAUO6', ' ', ' ', #385, #17682, $ ) ;
#21041 = NEXT_ASSEMBLY_USAGE_OCCURRENCE ( 'NAUO7', ' ', ' ', #385, #8857, $ ) ;
#21042 = NEXT_ASSEMBLY_USAGE_OCCURRENCE ( 'NAUO8', ' ', ' ', #385, #8857, $ ) ;
#21043 = NEXT_ASSEMBLY_USAGE_OCCURRENCE ( 'NAUO9', ' ', ' ', #385, #11075, $ ) ;
#21044 = NEXT_ASSEMBLY_USAGE_OCCURRENCE ( 'NAUO10', ' ', ' ', #385, #11075, $ ) ;
ENDSEC;
END-ISO-10303-21;
